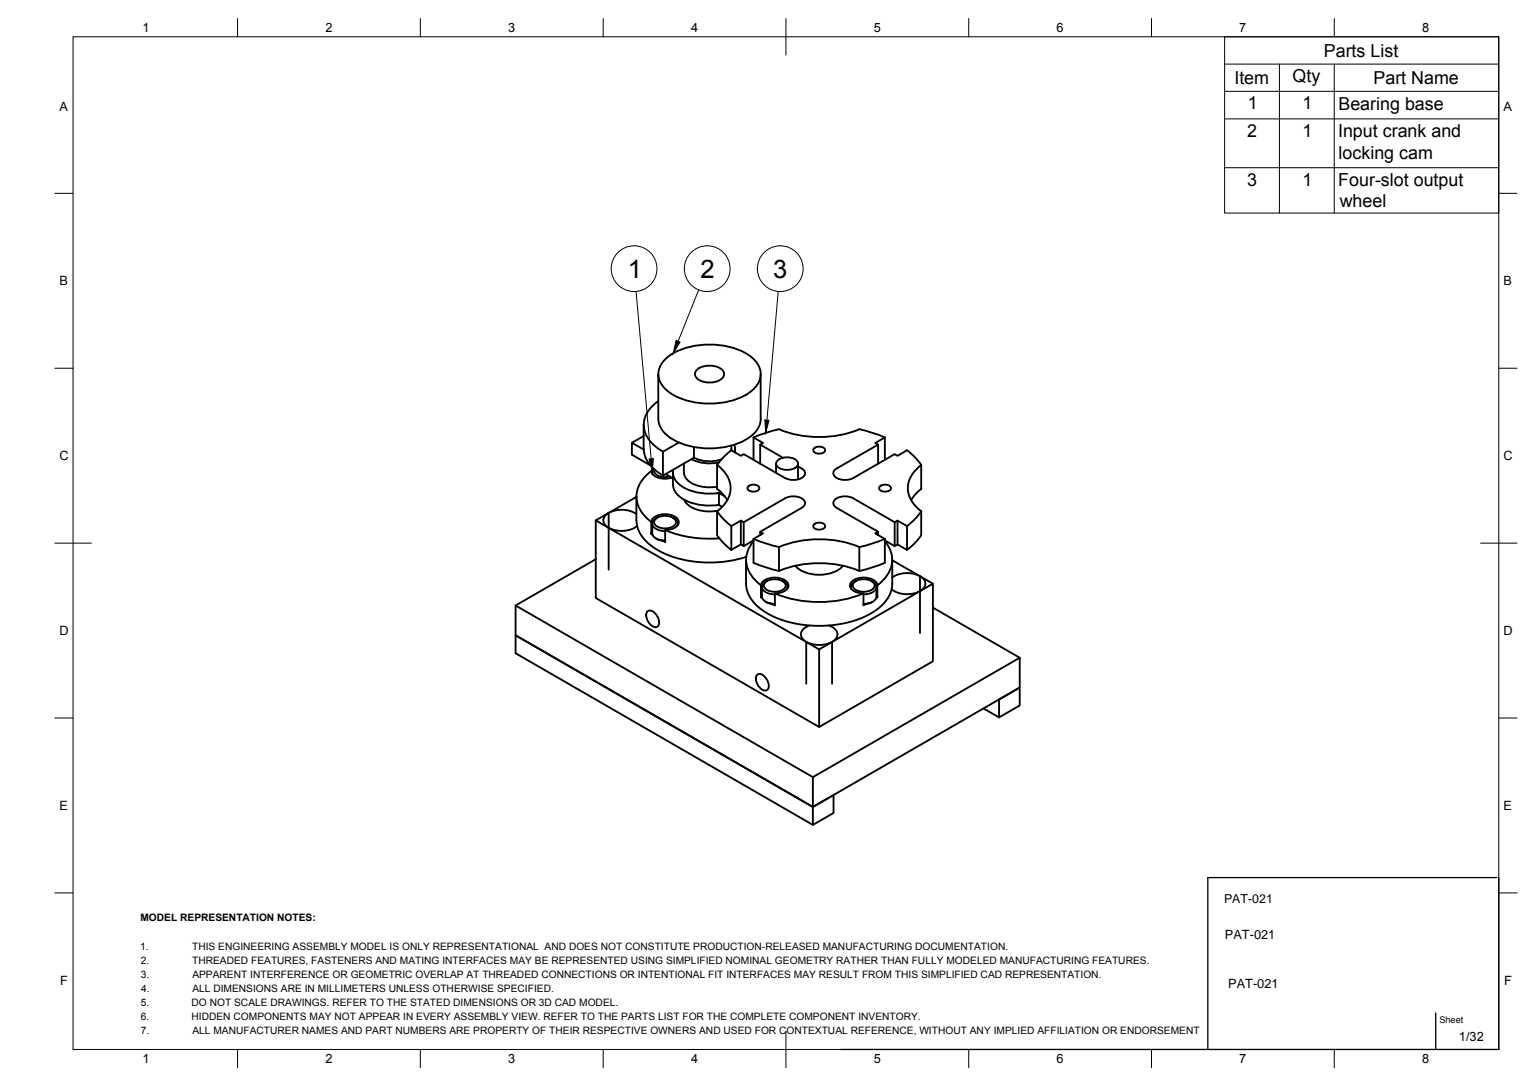
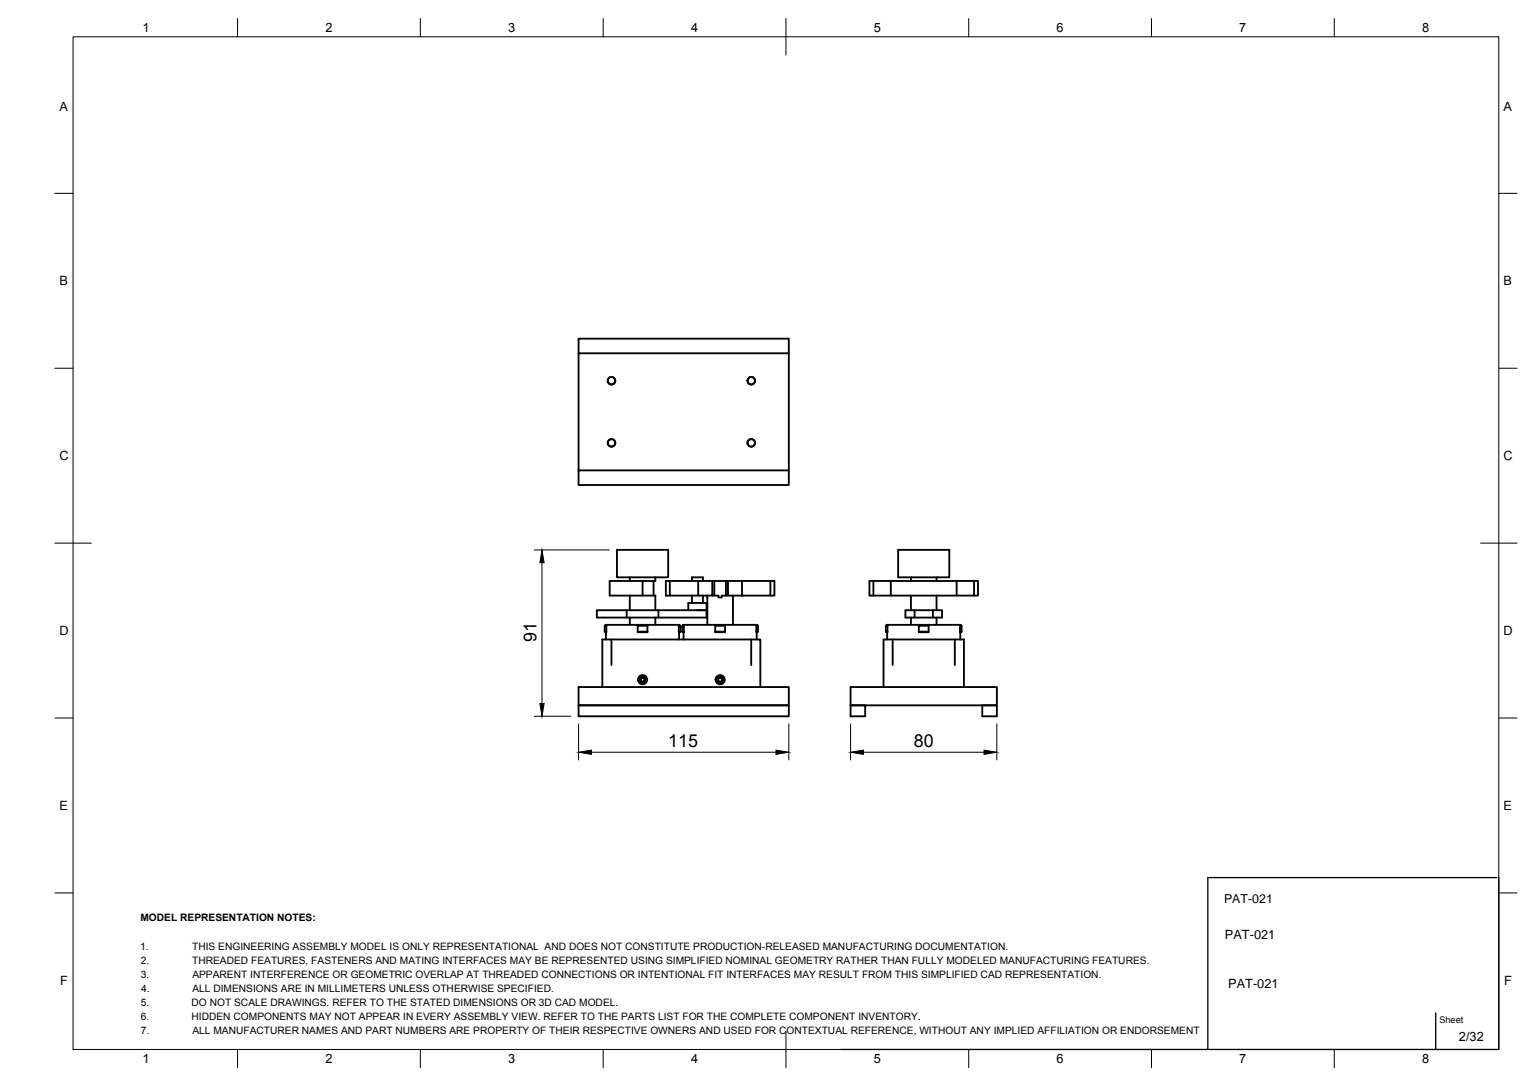
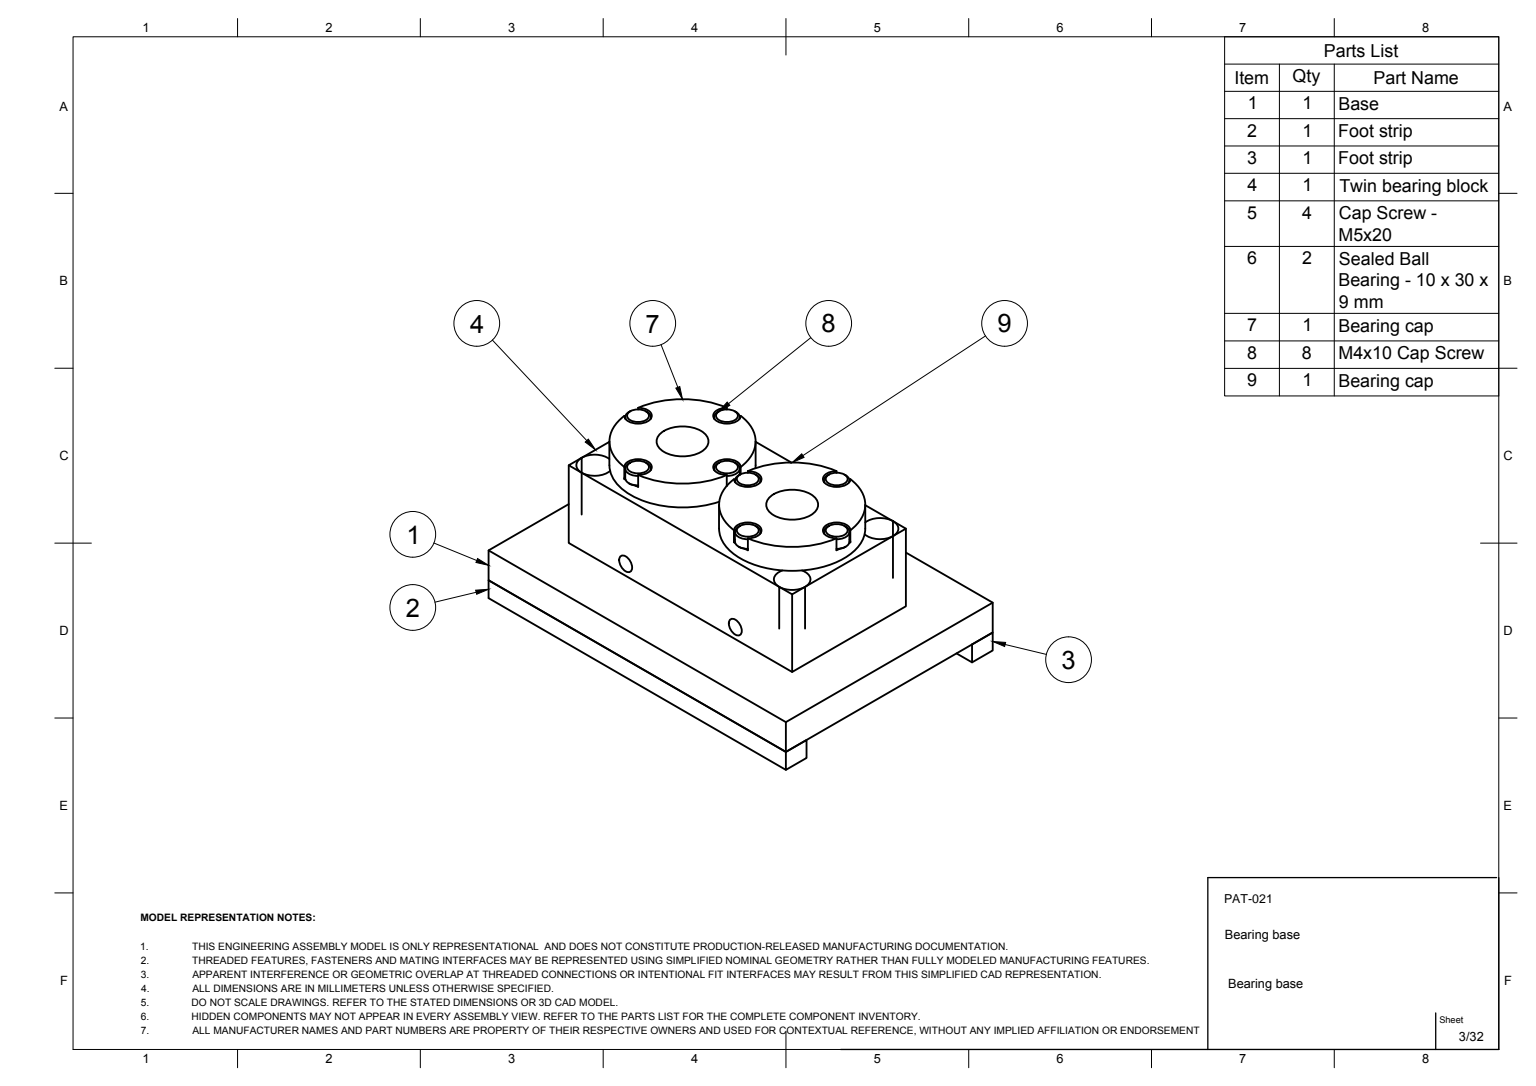
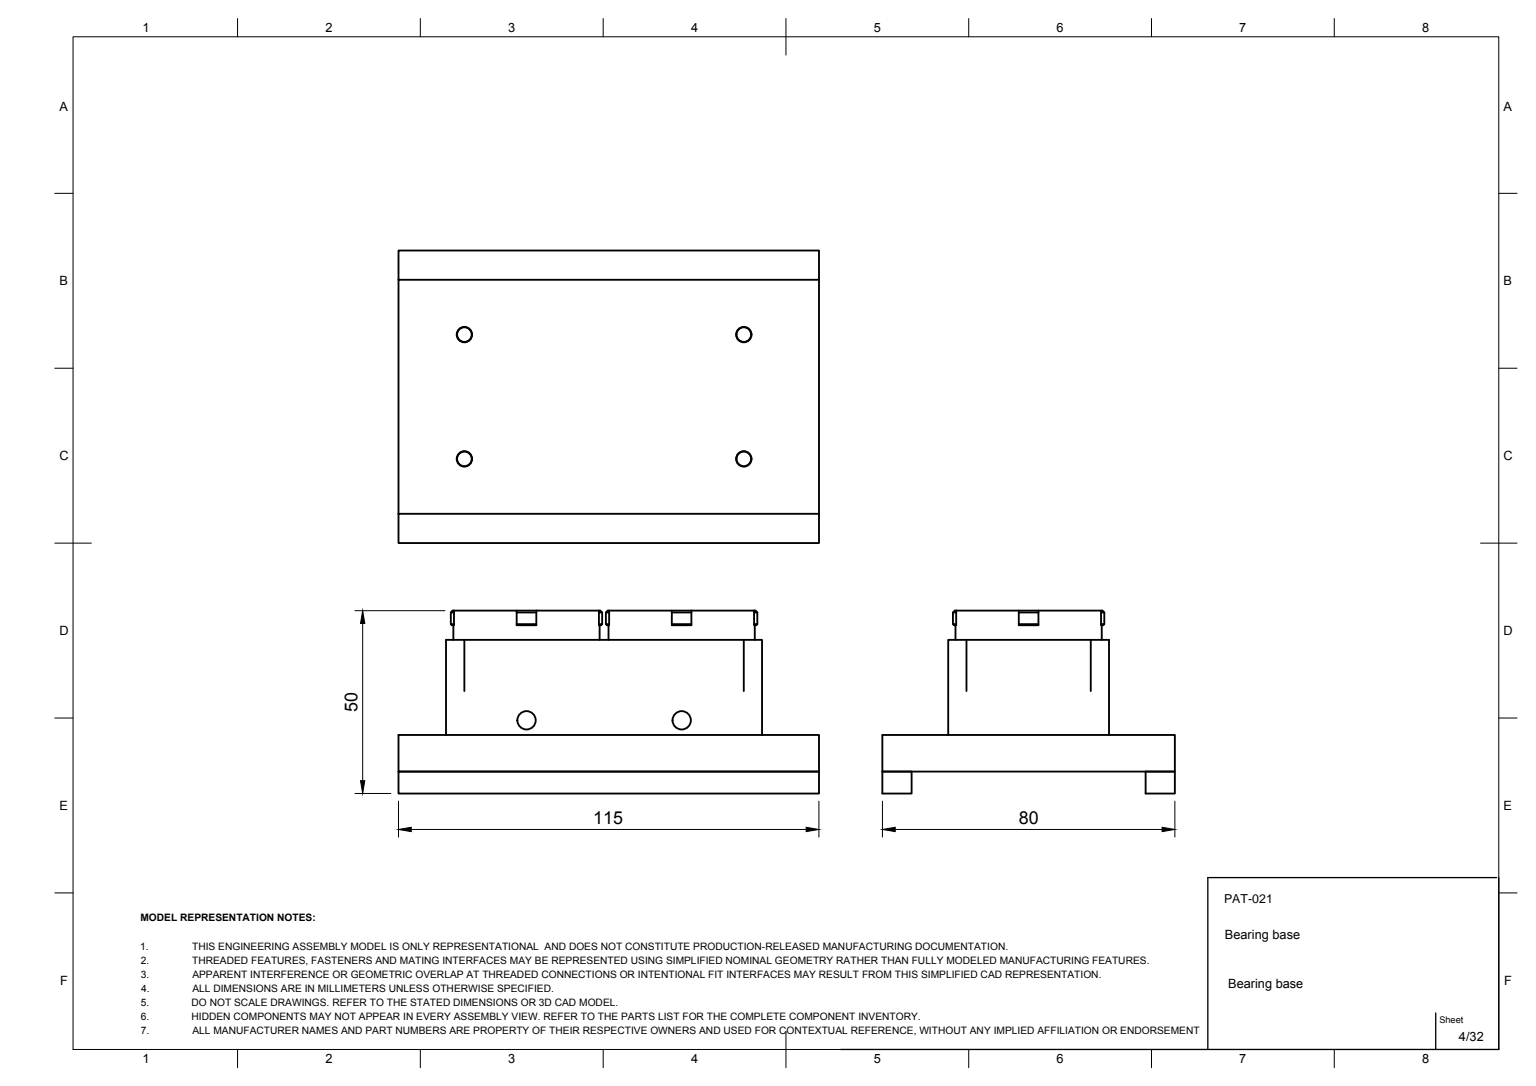
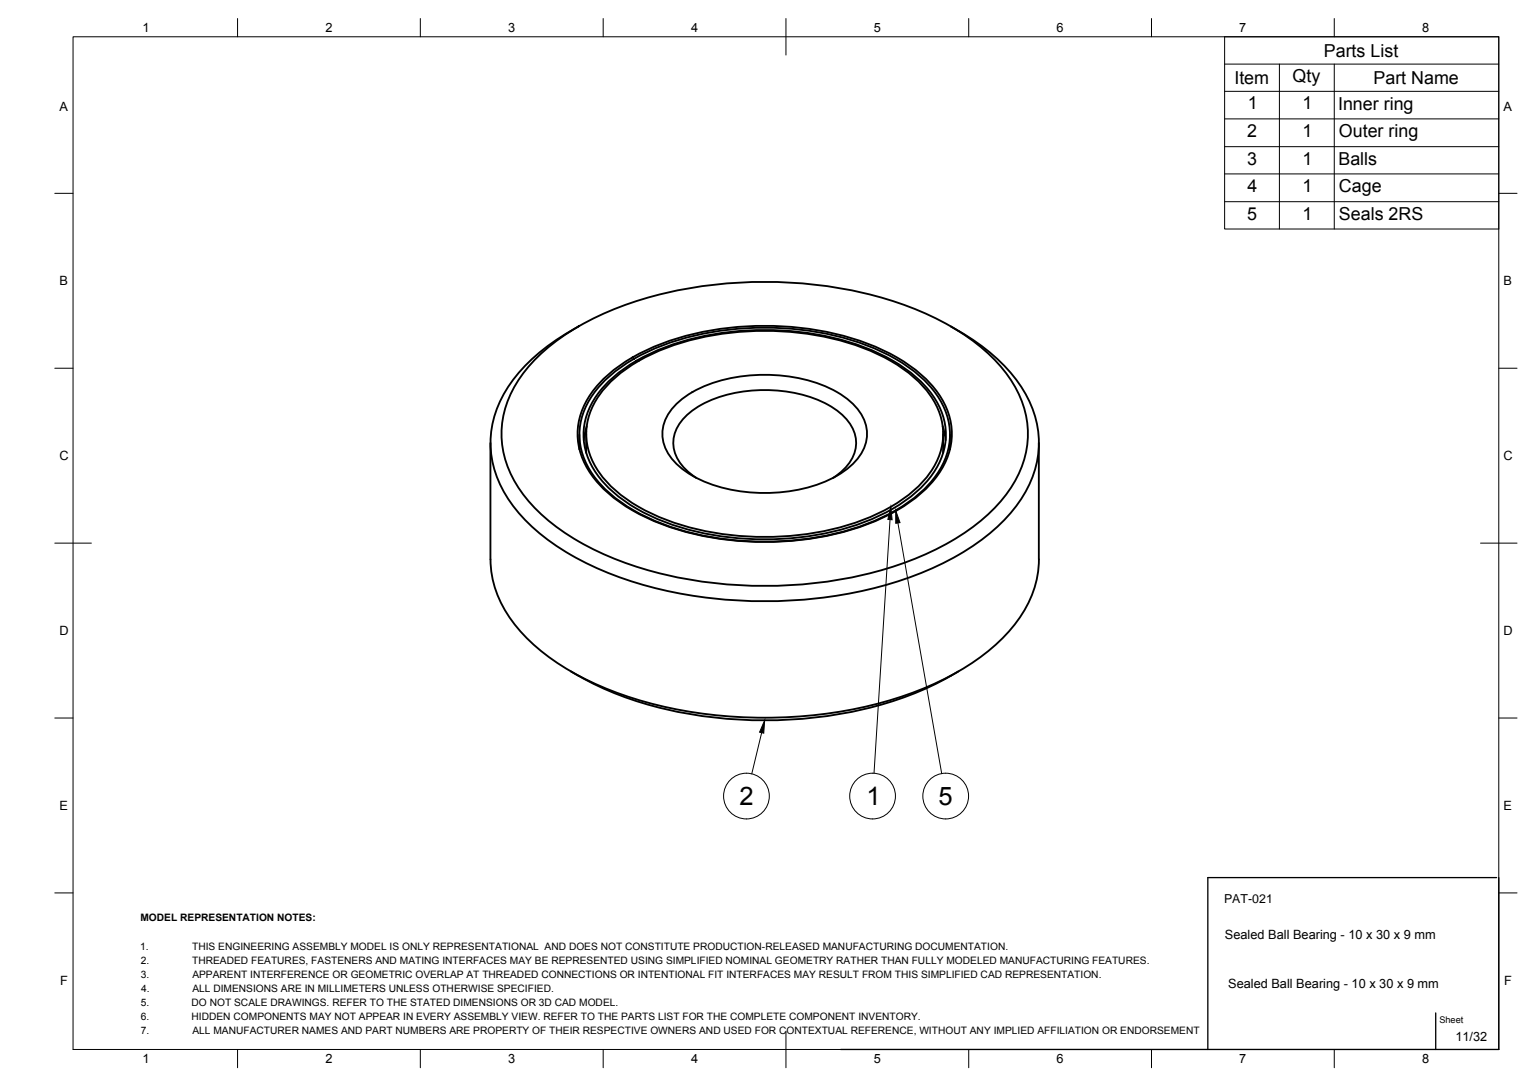
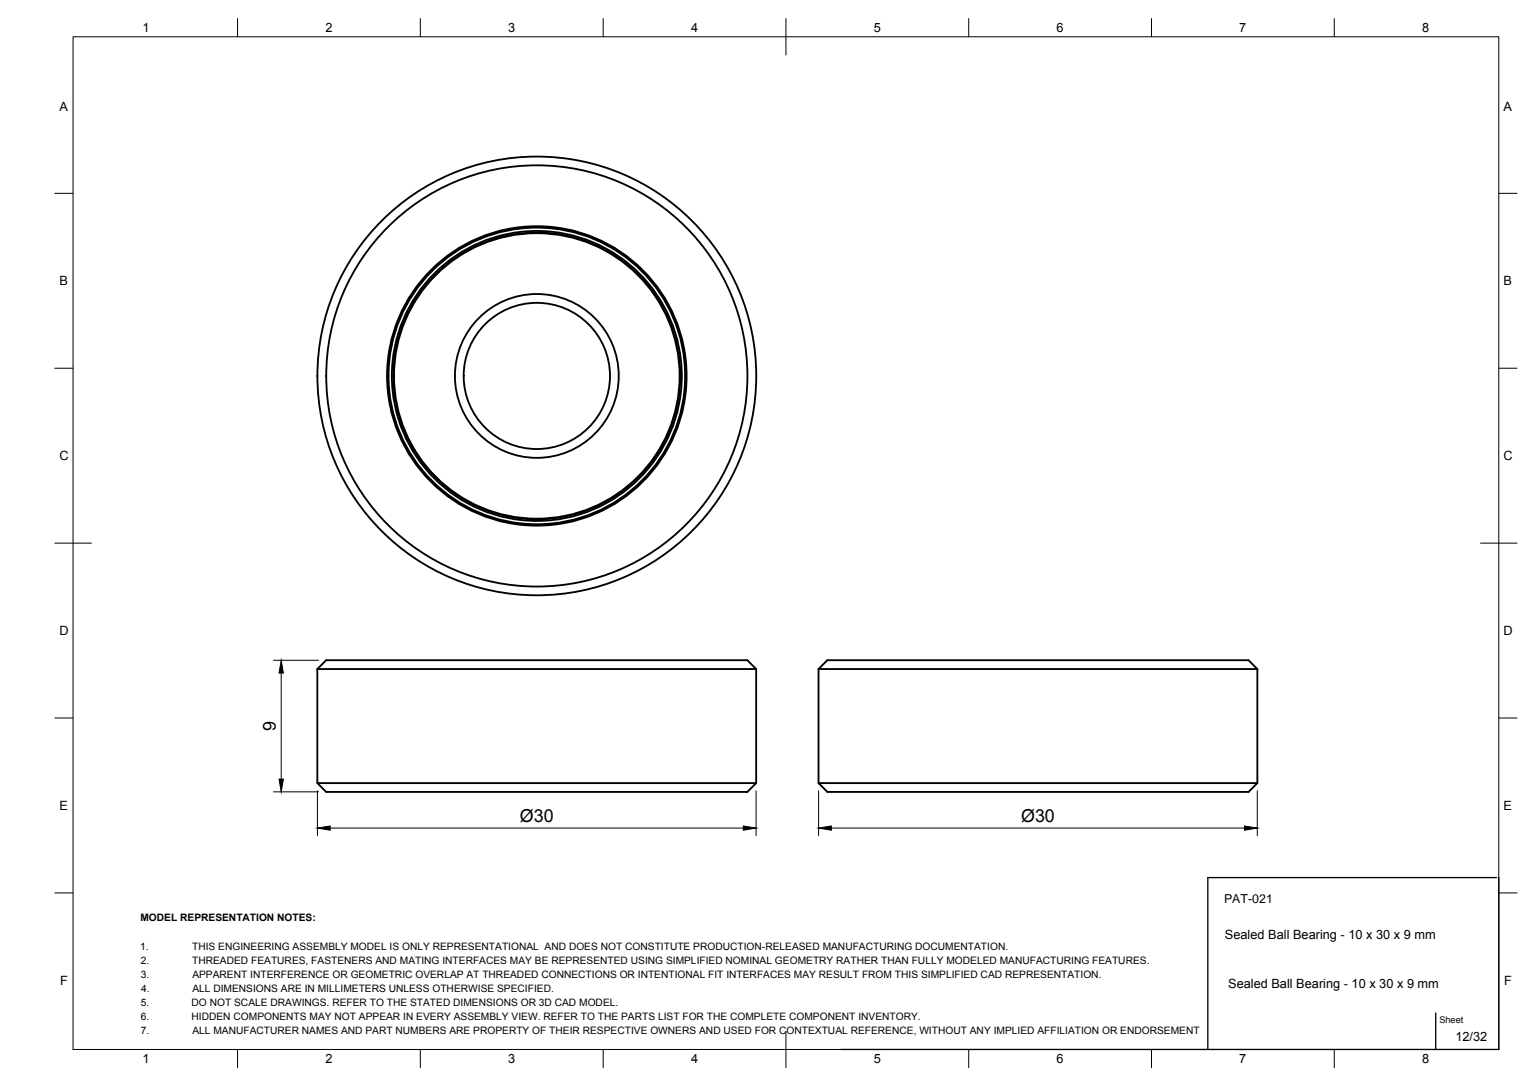
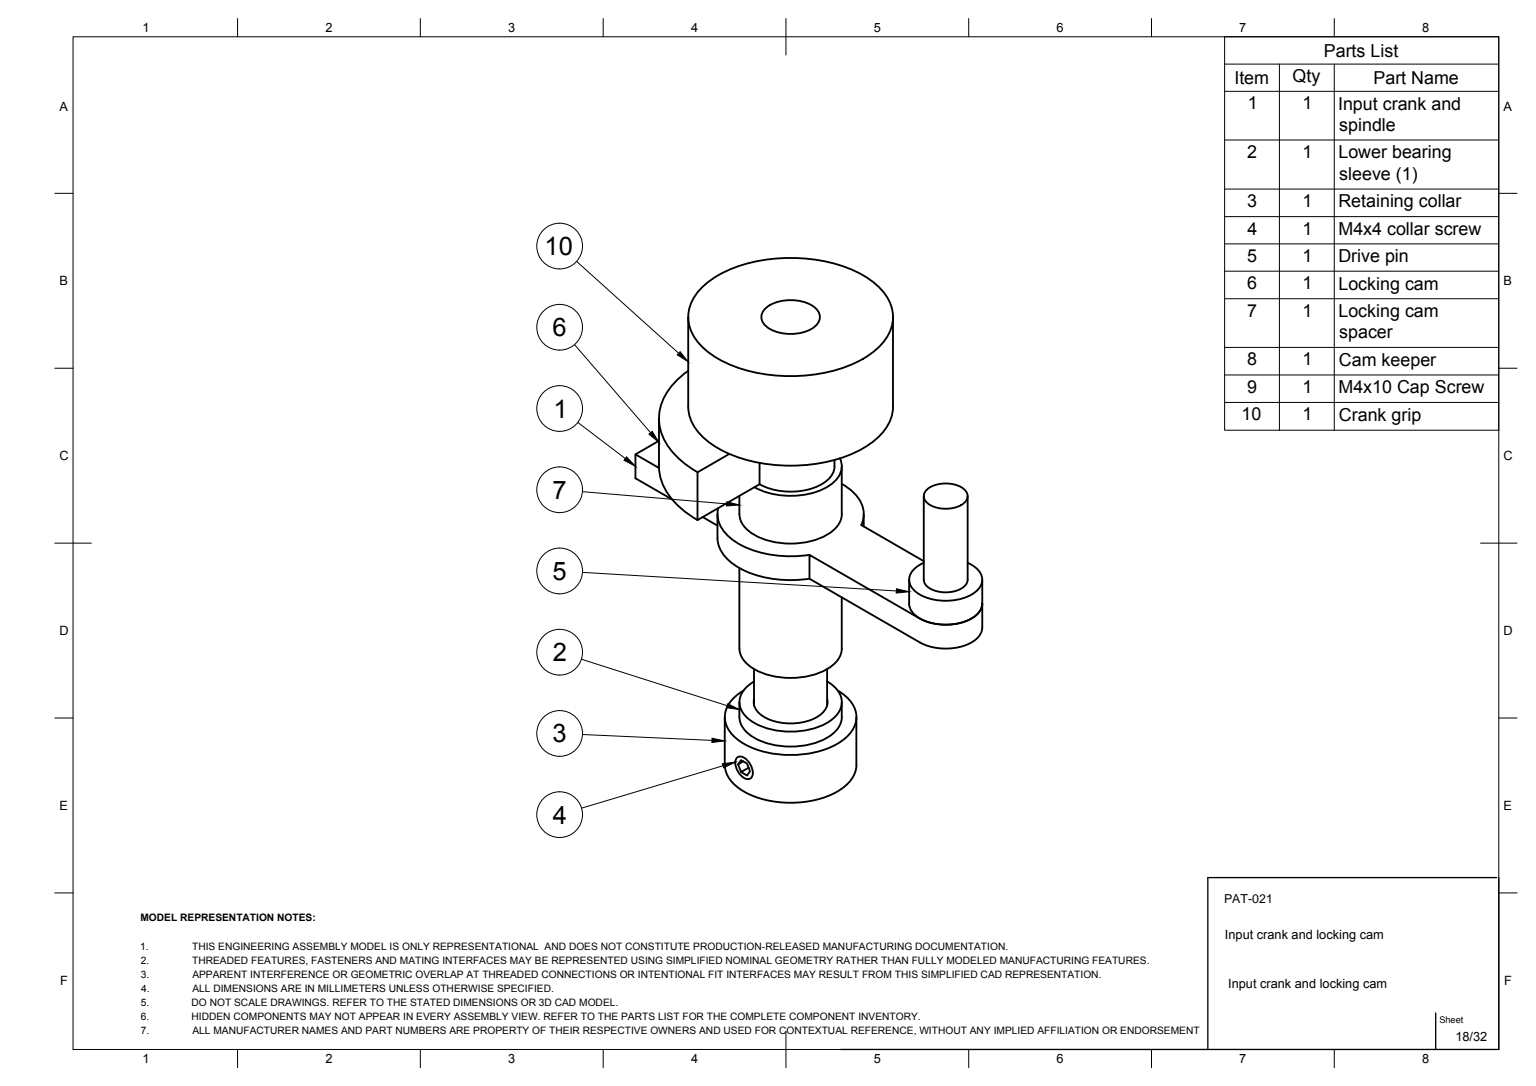
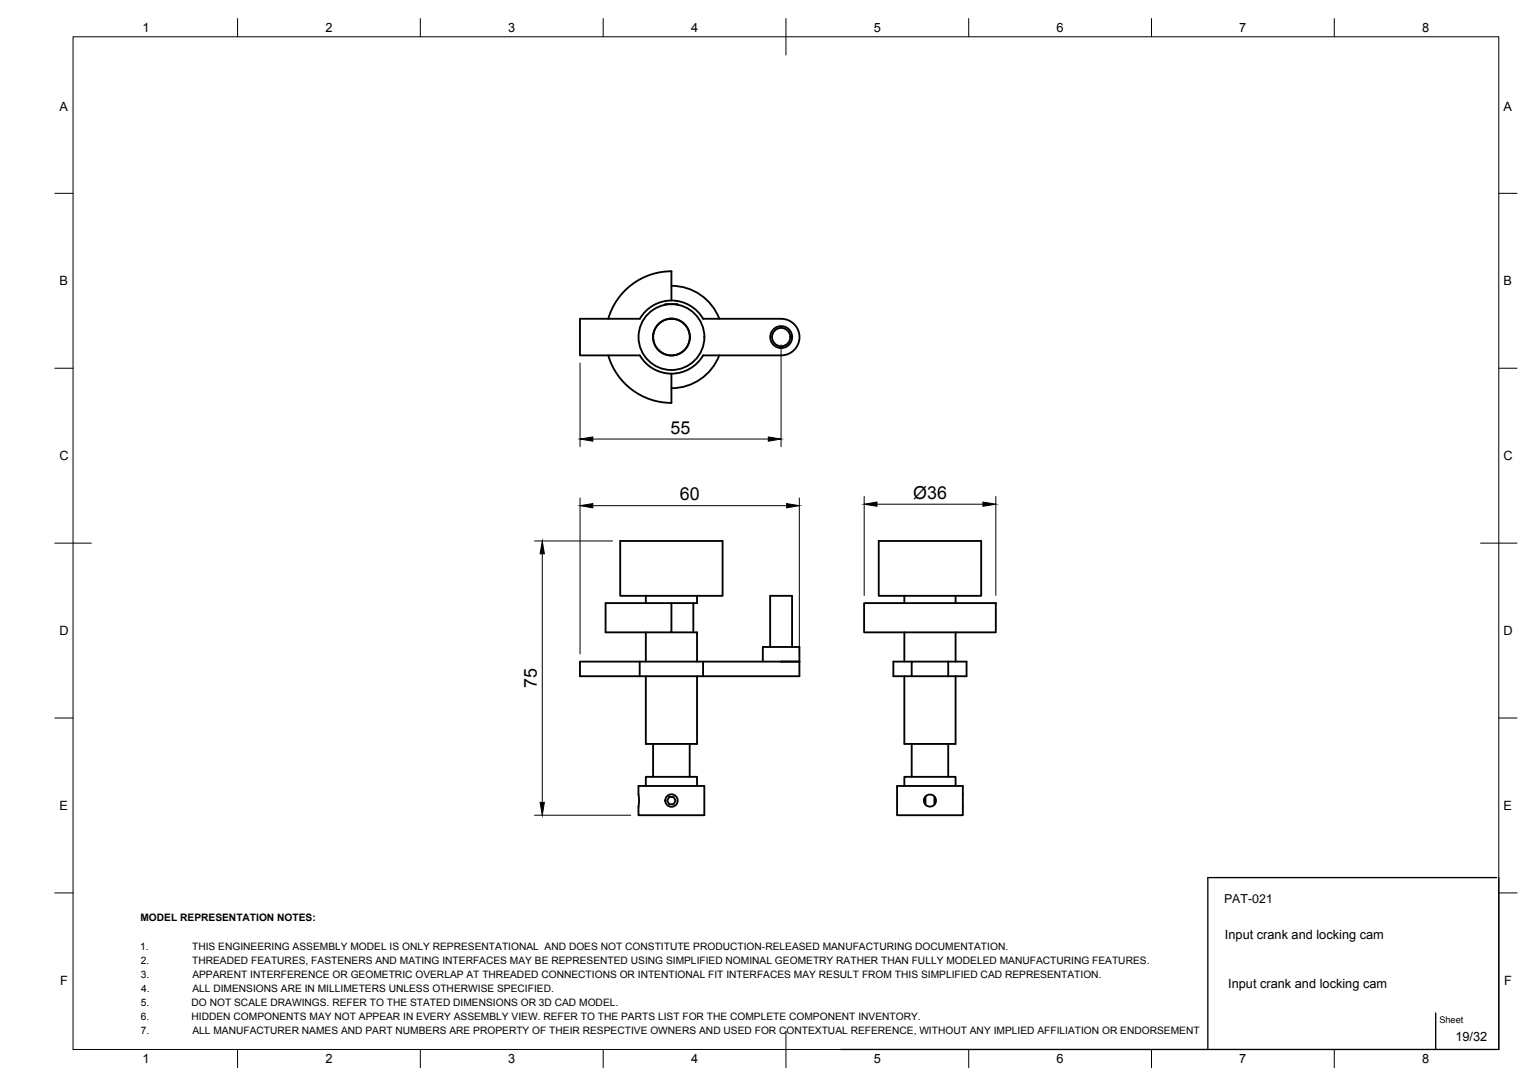
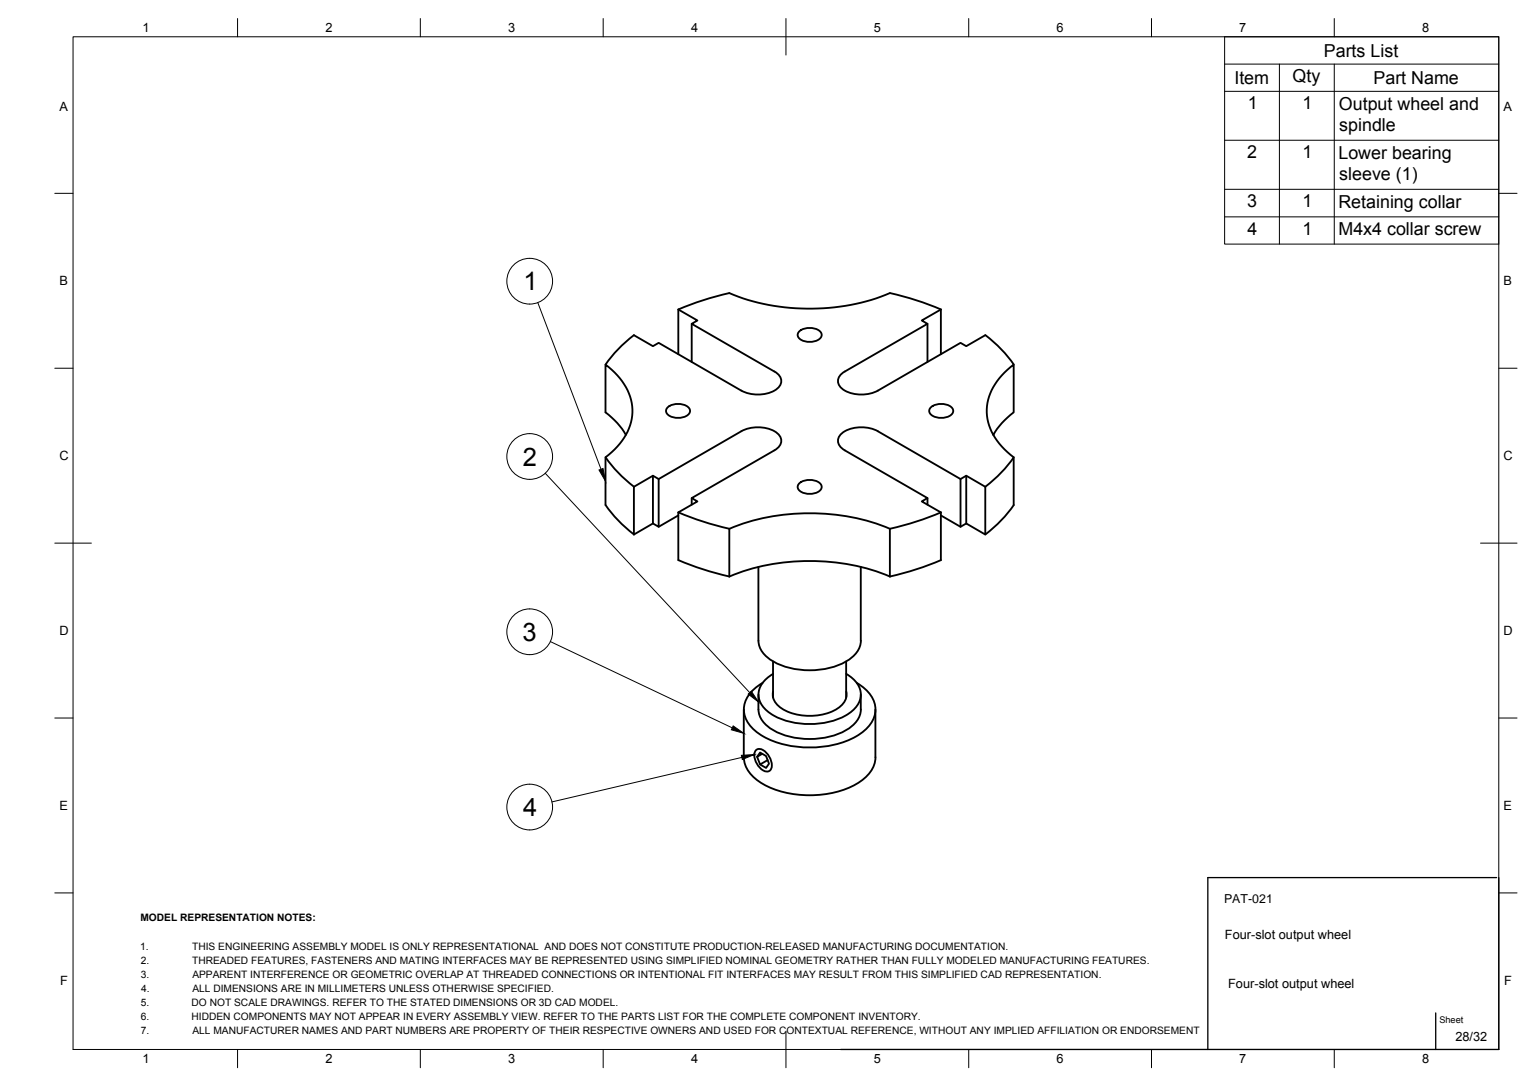
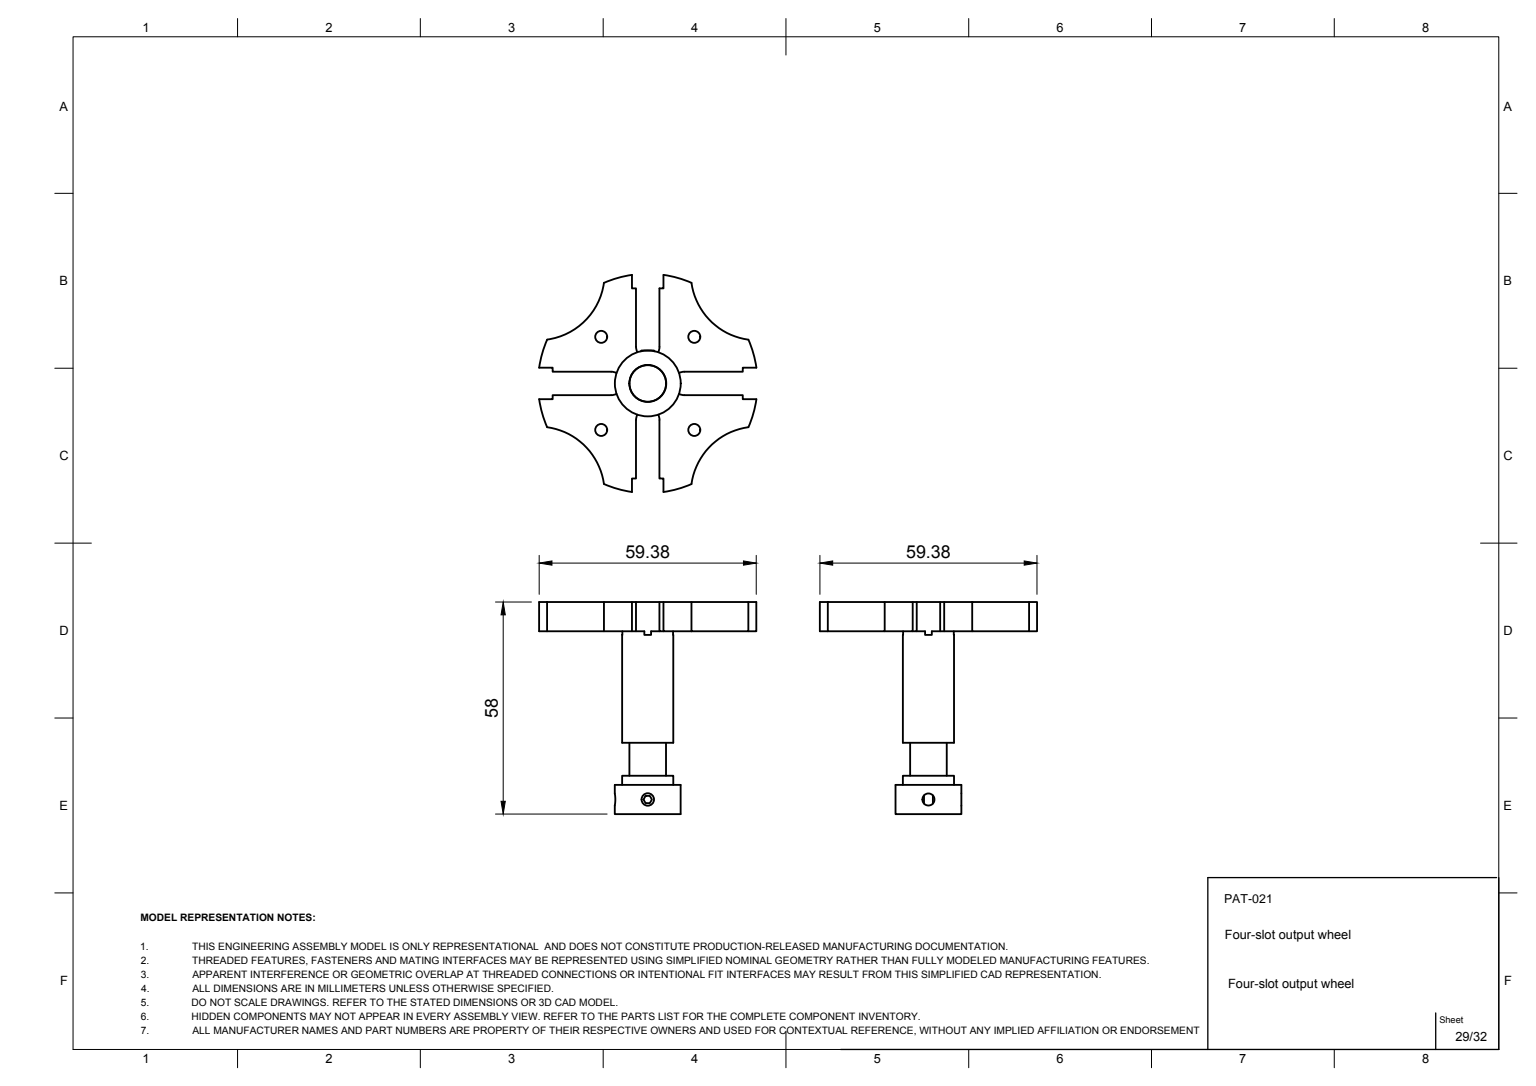
ISO-10303-21;
HEADER;
/* Generated by software containing ST-Developer
 * from STEP Tools, Inc. (www.steptools.com) 
 */

FILE_DESCRIPTION(
/* description */ ('Chain-less indexing wheel (Geneva) drive'),
/* implementation_level */ '2;1');

FILE_NAME(
/* name */ 'PAT-021',
/* time_stamp */ '2026-10-28T03:25:22-07:00',
/* author */ (''),
/* organization */ (''),
/* preprocessor_version */ 'ST-DEVELOPER v20.2',
/* originating_system */ 'Autodesk Translation Framework v15.17.0.0',
/* authorisation */ '');

FILE_SCHEMA (('AUTOMOTIVE_DESIGN { 1 0 10303 214 3 1 1 }'));
ENDSEC;

DATA;
#10=MECHANICAL_DESIGN_GEOMETRIC_PRESENTATION_REPRESENTATION('',(#303,#304,
#305,#306,#307,#308,#309,#310,#311,#312,#313,#314,#315,#316,#317,#318,#319,
#320,#321,#322,#323,#324,#325,#326,#327,#328,#329,#330,#331,#332,#333,#334,
#335),#10957);
#11=ITEM_DEFINED_TRANSFORMATION($,$,#6271,#6399);
#12=ITEM_DEFINED_TRANSFORMATION($,$,#6291,#6400);
#13=ITEM_DEFINED_TRANSFORMATION($,$,#6311,#6401);
#14=ITEM_DEFINED_TRANSFORMATION($,$,#6328,#6402);
#15=ITEM_DEFINED_TRANSFORMATION($,$,#6382,#6403);
#16=ITEM_DEFINED_TRANSFORMATION($,$,#6012,#6549);
#17=ITEM_DEFINED_TRANSFORMATION($,$,#6031,#6550);
#18=ITEM_DEFINED_TRANSFORMATION($,$,#6038,#6551);
#19=ITEM_DEFINED_TRANSFORMATION($,$,#6045,#6552);
#20=ITEM_DEFINED_TRANSFORMATION($,$,#6146,#6553);
#21=ITEM_DEFINED_TRANSFORMATION($,$,#6195,#6554);
#22=ITEM_DEFINED_TRANSFORMATION($,$,#6244,#6555);
#23=ITEM_DEFINED_TRANSFORMATION($,$,#6244,#6556);
#24=ITEM_DEFINED_TRANSFORMATION($,$,#6244,#6557);
#25=ITEM_DEFINED_TRANSFORMATION($,$,#6244,#6558);
#26=ITEM_DEFINED_TRANSFORMATION($,$,#6270,#6559);
#27=ITEM_DEFINED_TRANSFORMATION($,$,#6525,#6560);
#28=ITEM_DEFINED_TRANSFORMATION($,$,#6525,#6561);
#29=ITEM_DEFINED_TRANSFORMATION($,$,#6525,#6562);
#30=ITEM_DEFINED_TRANSFORMATION($,$,#6525,#6563);
#31=ITEM_DEFINED_TRANSFORMATION($,$,#6270,#6564);
#32=ITEM_DEFINED_TRANSFORMATION($,$,#6525,#6565);
#33=ITEM_DEFINED_TRANSFORMATION($,$,#6525,#6566);
#34=ITEM_DEFINED_TRANSFORMATION($,$,#6525,#6567);
#35=ITEM_DEFINED_TRANSFORMATION($,$,#6525,#6568);
#36=ITEM_DEFINED_TRANSFORMATION($,$,#6405,#6732);
#37=ITEM_DEFINED_TRANSFORMATION($,$,#6441,#6733);
#38=ITEM_DEFINED_TRANSFORMATION($,$,#6450,#6734);
#39=ITEM_DEFINED_TRANSFORMATION($,$,#6470,#6735);
#40=ITEM_DEFINED_TRANSFORMATION($,$,#6484,#6736);
#41=ITEM_DEFINED_TRANSFORMATION($,$,#6498,#6737);
#42=ITEM_DEFINED_TRANSFORMATION($,$,#6507,#6738);
#43=ITEM_DEFINED_TRANSFORMATION($,$,#6516,#6739);
#44=ITEM_DEFINED_TRANSFORMATION($,$,#6717,#6740);
#45=ITEM_DEFINED_TRANSFORMATION($,$,#6525,#6741);
#46=ITEM_DEFINED_TRANSFORMATION($,$,#6570,#6742);
#47=ITEM_DEFINED_TRANSFORMATION($,$,#6688,#6743);
#48=ITEM_DEFINED_TRANSFORMATION($,$,#6697,#6744);
#49=ITEM_DEFINED_TRANSFORMATION($,$,#6717,#6745);
#50=ITEM_DEFINED_TRANSFORMATION($,$,#6011,#6746);
#51=ITEM_DEFINED_TRANSFORMATION($,$,#6404,#6747);
#52=ITEM_DEFINED_TRANSFORMATION($,$,#6569,#6748);
#53=(
REPRESENTATION_RELATIONSHIP($,$,#11074,#11073)
REPRESENTATION_RELATIONSHIP_WITH_TRANSFORMATION(#11)
SHAPE_REPRESENTATION_RELATIONSHIP()
);
#54=(
REPRESENTATION_RELATIONSHIP($,$,#11075,#11073)
REPRESENTATION_RELATIONSHIP_WITH_TRANSFORMATION(#12)
SHAPE_REPRESENTATION_RELATIONSHIP()
);
#55=(
REPRESENTATION_RELATIONSHIP($,$,#11076,#11073)
REPRESENTATION_RELATIONSHIP_WITH_TRANSFORMATION(#13)
SHAPE_REPRESENTATION_RELATIONSHIP()
);
#56=(
REPRESENTATION_RELATIONSHIP($,$,#11077,#11073)
REPRESENTATION_RELATIONSHIP_WITH_TRANSFORMATION(#14)
SHAPE_REPRESENTATION_RELATIONSHIP()
);
#57=(
REPRESENTATION_RELATIONSHIP($,$,#11078,#11073)
REPRESENTATION_RELATIONSHIP_WITH_TRANSFORMATION(#15)
SHAPE_REPRESENTATION_RELATIONSHIP()
);
#58=(
REPRESENTATION_RELATIONSHIP($,$,#11066,#11065)
REPRESENTATION_RELATIONSHIP_WITH_TRANSFORMATION(#16)
SHAPE_REPRESENTATION_RELATIONSHIP()
);
#59=(
REPRESENTATION_RELATIONSHIP($,$,#11067,#11065)
REPRESENTATION_RELATIONSHIP_WITH_TRANSFORMATION(#17)
SHAPE_REPRESENTATION_RELATIONSHIP()
);
#60=(
REPRESENTATION_RELATIONSHIP($,$,#11068,#11065)
REPRESENTATION_RELATIONSHIP_WITH_TRANSFORMATION(#18)
SHAPE_REPRESENTATION_RELATIONSHIP()
);
#61=(
REPRESENTATION_RELATIONSHIP($,$,#11069,#11065)
REPRESENTATION_RELATIONSHIP_WITH_TRANSFORMATION(#19)
SHAPE_REPRESENTATION_RELATIONSHIP()
);
#62=(
REPRESENTATION_RELATIONSHIP($,$,#11070,#11065)
REPRESENTATION_RELATIONSHIP_WITH_TRANSFORMATION(#20)
SHAPE_REPRESENTATION_RELATIONSHIP()
);
#63=(
REPRESENTATION_RELATIONSHIP($,$,#11071,#11065)
REPRESENTATION_RELATIONSHIP_WITH_TRANSFORMATION(#21)
SHAPE_REPRESENTATION_RELATIONSHIP()
);
#64=(
REPRESENTATION_RELATIONSHIP($,$,#11072,#11065)
REPRESENTATION_RELATIONSHIP_WITH_TRANSFORMATION(#22)
SHAPE_REPRESENTATION_RELATIONSHIP()
);
#65=(
REPRESENTATION_RELATIONSHIP($,$,#11072,#11065)
REPRESENTATION_RELATIONSHIP_WITH_TRANSFORMATION(#23)
SHAPE_REPRESENTATION_RELATIONSHIP()
);
#66=(
REPRESENTATION_RELATIONSHIP($,$,#11072,#11065)
REPRESENTATION_RELATIONSHIP_WITH_TRANSFORMATION(#24)
SHAPE_REPRESENTATION_RELATIONSHIP()
);
#67=(
REPRESENTATION_RELATIONSHIP($,$,#11072,#11065)
REPRESENTATION_RELATIONSHIP_WITH_TRANSFORMATION(#25)
SHAPE_REPRESENTATION_RELATIONSHIP()
);
#68=(
REPRESENTATION_RELATIONSHIP($,$,#11073,#11065)
REPRESENTATION_RELATIONSHIP_WITH_TRANSFORMATION(#26)
SHAPE_REPRESENTATION_RELATIONSHIP()
);
#69=(
REPRESENTATION_RELATIONSHIP($,$,#11088,#11065)
REPRESENTATION_RELATIONSHIP_WITH_TRANSFORMATION(#27)
SHAPE_REPRESENTATION_RELATIONSHIP()
);
#70=(
REPRESENTATION_RELATIONSHIP($,$,#11088,#11065)
REPRESENTATION_RELATIONSHIP_WITH_TRANSFORMATION(#28)
SHAPE_REPRESENTATION_RELATIONSHIP()
);
#71=(
REPRESENTATION_RELATIONSHIP($,$,#11088,#11065)
REPRESENTATION_RELATIONSHIP_WITH_TRANSFORMATION(#29)
SHAPE_REPRESENTATION_RELATIONSHIP()
);
#72=(
REPRESENTATION_RELATIONSHIP($,$,#11088,#11065)
REPRESENTATION_RELATIONSHIP_WITH_TRANSFORMATION(#30)
SHAPE_REPRESENTATION_RELATIONSHIP()
);
#73=(
REPRESENTATION_RELATIONSHIP($,$,#11073,#11065)
REPRESENTATION_RELATIONSHIP_WITH_TRANSFORMATION(#31)
SHAPE_REPRESENTATION_RELATIONSHIP()
);
#74=(
REPRESENTATION_RELATIONSHIP($,$,#11088,#11065)
REPRESENTATION_RELATIONSHIP_WITH_TRANSFORMATION(#32)
SHAPE_REPRESENTATION_RELATIONSHIP()
);
#75=(
REPRESENTATION_RELATIONSHIP($,$,#11088,#11065)
REPRESENTATION_RELATIONSHIP_WITH_TRANSFORMATION(#33)
SHAPE_REPRESENTATION_RELATIONSHIP()
);
#76=(
REPRESENTATION_RELATIONSHIP($,$,#11088,#11065)
REPRESENTATION_RELATIONSHIP_WITH_TRANSFORMATION(#34)
SHAPE_REPRESENTATION_RELATIONSHIP()
);
#77=(
REPRESENTATION_RELATIONSHIP($,$,#11088,#11065)
REPRESENTATION_RELATIONSHIP_WITH_TRANSFORMATION(#35)
SHAPE_REPRESENTATION_RELATIONSHIP()
);
#78=(
REPRESENTATION_RELATIONSHIP($,$,#11080,#11079)
REPRESENTATION_RELATIONSHIP_WITH_TRANSFORMATION(#36)
SHAPE_REPRESENTATION_RELATIONSHIP()
);
#79=(
REPRESENTATION_RELATIONSHIP($,$,#11081,#11079)
REPRESENTATION_RELATIONSHIP_WITH_TRANSFORMATION(#37)
SHAPE_REPRESENTATION_RELATIONSHIP()
);
#80=(
REPRESENTATION_RELATIONSHIP($,$,#11082,#11079)
REPRESENTATION_RELATIONSHIP_WITH_TRANSFORMATION(#38)
SHAPE_REPRESENTATION_RELATIONSHIP()
);
#81=(
REPRESENTATION_RELATIONSHIP($,$,#11083,#11079)
REPRESENTATION_RELATIONSHIP_WITH_TRANSFORMATION(#39)
SHAPE_REPRESENTATION_RELATIONSHIP()
);
#82=(
REPRESENTATION_RELATIONSHIP($,$,#11084,#11079)
REPRESENTATION_RELATIONSHIP_WITH_TRANSFORMATION(#40)
SHAPE_REPRESENTATION_RELATIONSHIP()
);
#83=(
REPRESENTATION_RELATIONSHIP($,$,#11085,#11079)
REPRESENTATION_RELATIONSHIP_WITH_TRANSFORMATION(#41)
SHAPE_REPRESENTATION_RELATIONSHIP()
);
#84=(
REPRESENTATION_RELATIONSHIP($,$,#11086,#11079)
REPRESENTATION_RELATIONSHIP_WITH_TRANSFORMATION(#42)
SHAPE_REPRESENTATION_RELATIONSHIP()
);
#85=(
REPRESENTATION_RELATIONSHIP($,$,#11087,#11079)
REPRESENTATION_RELATIONSHIP_WITH_TRANSFORMATION(#43)
SHAPE_REPRESENTATION_RELATIONSHIP()
);
#86=(
REPRESENTATION_RELATIONSHIP($,$,#11093,#11079)
REPRESENTATION_RELATIONSHIP_WITH_TRANSFORMATION(#44)
SHAPE_REPRESENTATION_RELATIONSHIP()
);
#87=(
REPRESENTATION_RELATIONSHIP($,$,#11088,#11079)
REPRESENTATION_RELATIONSHIP_WITH_TRANSFORMATION(#45)
SHAPE_REPRESENTATION_RELATIONSHIP()
);
#88=(
REPRESENTATION_RELATIONSHIP($,$,#11090,#11089)
REPRESENTATION_RELATIONSHIP_WITH_TRANSFORMATION(#46)
SHAPE_REPRESENTATION_RELATIONSHIP()
);
#89=(
REPRESENTATION_RELATIONSHIP($,$,#11091,#11089)
REPRESENTATION_RELATIONSHIP_WITH_TRANSFORMATION(#47)
SHAPE_REPRESENTATION_RELATIONSHIP()
);
#90=(
REPRESENTATION_RELATIONSHIP($,$,#11092,#11089)
REPRESENTATION_RELATIONSHIP_WITH_TRANSFORMATION(#48)
SHAPE_REPRESENTATION_RELATIONSHIP()
);
#91=(
REPRESENTATION_RELATIONSHIP($,$,#11093,#11089)
REPRESENTATION_RELATIONSHIP_WITH_TRANSFORMATION(#49)
SHAPE_REPRESENTATION_RELATIONSHIP()
);
#92=(
REPRESENTATION_RELATIONSHIP($,$,#11065,#11064)
REPRESENTATION_RELATIONSHIP_WITH_TRANSFORMATION(#50)
SHAPE_REPRESENTATION_RELATIONSHIP()
);
#93=(
REPRESENTATION_RELATIONSHIP($,$,#11079,#11064)
REPRESENTATION_RELATIONSHIP_WITH_TRANSFORMATION(#51)
SHAPE_REPRESENTATION_RELATIONSHIP()
);
#94=(
REPRESENTATION_RELATIONSHIP($,$,#11089,#11064)
REPRESENTATION_RELATIONSHIP_WITH_TRANSFORMATION(#52)
SHAPE_REPRESENTATION_RELATIONSHIP()
);
#95=CONTEXT_DEPENDENT_SHAPE_REPRESENTATION(#53,#11007);
#96=CONTEXT_DEPENDENT_SHAPE_REPRESENTATION(#54,#11008);
#97=CONTEXT_DEPENDENT_SHAPE_REPRESENTATION(#55,#11009);
#98=CONTEXT_DEPENDENT_SHAPE_REPRESENTATION(#56,#11010);
#99=CONTEXT_DEPENDENT_SHAPE_REPRESENTATION(#57,#11011);
#100=CONTEXT_DEPENDENT_SHAPE_REPRESENTATION(#58,#11022);
#101=CONTEXT_DEPENDENT_SHAPE_REPRESENTATION(#59,#11023);
#102=CONTEXT_DEPENDENT_SHAPE_REPRESENTATION(#60,#11024);
#103=CONTEXT_DEPENDENT_SHAPE_REPRESENTATION(#61,#11025);
#104=CONTEXT_DEPENDENT_SHAPE_REPRESENTATION(#62,#11026);
#105=CONTEXT_DEPENDENT_SHAPE_REPRESENTATION(#63,#11027);
#106=CONTEXT_DEPENDENT_SHAPE_REPRESENTATION(#64,#11028);
#107=CONTEXT_DEPENDENT_SHAPE_REPRESENTATION(#65,#11029);
#108=CONTEXT_DEPENDENT_SHAPE_REPRESENTATION(#66,#11030);
#109=CONTEXT_DEPENDENT_SHAPE_REPRESENTATION(#67,#11031);
#110=CONTEXT_DEPENDENT_SHAPE_REPRESENTATION(#68,#11032);
#111=CONTEXT_DEPENDENT_SHAPE_REPRESENTATION(#69,#11033);
#112=CONTEXT_DEPENDENT_SHAPE_REPRESENTATION(#70,#11034);
#113=CONTEXT_DEPENDENT_SHAPE_REPRESENTATION(#71,#11035);
#114=CONTEXT_DEPENDENT_SHAPE_REPRESENTATION(#72,#11036);
#115=CONTEXT_DEPENDENT_SHAPE_REPRESENTATION(#73,#11037);
#116=CONTEXT_DEPENDENT_SHAPE_REPRESENTATION(#74,#11038);
#117=CONTEXT_DEPENDENT_SHAPE_REPRESENTATION(#75,#11039);
#118=CONTEXT_DEPENDENT_SHAPE_REPRESENTATION(#76,#11040);
#119=CONTEXT_DEPENDENT_SHAPE_REPRESENTATION(#77,#11041);
#120=CONTEXT_DEPENDENT_SHAPE_REPRESENTATION(#78,#11047);
#121=CONTEXT_DEPENDENT_SHAPE_REPRESENTATION(#79,#11048);
#122=CONTEXT_DEPENDENT_SHAPE_REPRESENTATION(#80,#11049);
#123=CONTEXT_DEPENDENT_SHAPE_REPRESENTATION(#81,#11050);
#124=CONTEXT_DEPENDENT_SHAPE_REPRESENTATION(#82,#11051);
#125=CONTEXT_DEPENDENT_SHAPE_REPRESENTATION(#83,#11052);
#126=CONTEXT_DEPENDENT_SHAPE_REPRESENTATION(#84,#11053);
#127=CONTEXT_DEPENDENT_SHAPE_REPRESENTATION(#85,#11054);
#128=CONTEXT_DEPENDENT_SHAPE_REPRESENTATION(#86,#11055);
#129=CONTEXT_DEPENDENT_SHAPE_REPRESENTATION(#87,#11056);
#130=CONTEXT_DEPENDENT_SHAPE_REPRESENTATION(#88,#11057);
#131=CONTEXT_DEPENDENT_SHAPE_REPRESENTATION(#89,#11058);
#132=CONTEXT_DEPENDENT_SHAPE_REPRESENTATION(#90,#11059);
#133=CONTEXT_DEPENDENT_SHAPE_REPRESENTATION(#91,#11060);
#134=CONTEXT_DEPENDENT_SHAPE_REPRESENTATION(#92,#11061);
#135=CONTEXT_DEPENDENT_SHAPE_REPRESENTATION(#93,#11062);
#136=CONTEXT_DEPENDENT_SHAPE_REPRESENTATION(#94,#11063);
#137=NEXT_ASSEMBLY_USAGE_OCCURRENCE('Inner ring:1','Inner ring:1',
'Inner ring:1',#11104,#11105,'Inner ring:1');
#138=NEXT_ASSEMBLY_USAGE_OCCURRENCE('Outer ring:1','Outer ring:1',
'Outer ring:1',#11104,#11106,'Outer ring:1');
#139=NEXT_ASSEMBLY_USAGE_OCCURRENCE('Balls:1','Balls:1','Balls:1',#11104,
#11107,'Balls:1');
#140=NEXT_ASSEMBLY_USAGE_OCCURRENCE('Cage:1','Cage:1','Cage:1',#11104,#11108,
'Cage:1');
#141=NEXT_ASSEMBLY_USAGE_OCCURRENCE('Seals 2RS:1','Seals 2RS:1',
'Seals 2RS:1',#11104,#11109,'Seals 2RS:1');
#142=NEXT_ASSEMBLY_USAGE_OCCURRENCE('Base:1','Base:1','Base:1',#11096,#11097,
'Base:1');
#143=NEXT_ASSEMBLY_USAGE_OCCURRENCE('Foot strip:1','Foot strip:1',
'Foot strip:1',#11096,#11098,'Foot strip:1');
#144=NEXT_ASSEMBLY_USAGE_OCCURRENCE('Foot strip (1):1',
'Foot strip (1):1','Foot strip (1):1',#11096,#11099,'Foot strip (1):1');
#145=NEXT_ASSEMBLY_USAGE_OCCURRENCE('Twin bearing block:1',
'Twin bearing block:1','Twin bearing block:1',#11096,#11100,
'Twin bearing block:1');
#146=NEXT_ASSEMBLY_USAGE_OCCURRENCE('Bearing cap:1','Bearing cap:1',
'Bearing cap:1',#11096,#11101,'Bearing cap:1');
#147=NEXT_ASSEMBLY_USAGE_OCCURRENCE('Bearing cap (1):1',
'Bearing cap (1):1','Bearing cap (1):1',#11096,#11102,
'Bearing cap (1):1');
#148=NEXT_ASSEMBLY_USAGE_OCCURRENCE('Cap Screw - M5x20:2',
'Cap Screw - M5x20:2','Cap Screw - M5x20:2',#11096,#11103,
'Cap Screw - M5x20:2');
#149=NEXT_ASSEMBLY_USAGE_OCCURRENCE('Cap Screw - M5x20:3',
'Cap Screw - M5x20:3','Cap Screw - M5x20:3',#11096,#11103,
'Cap Screw - M5x20:3');
#150=NEXT_ASSEMBLY_USAGE_OCCURRENCE('Cap Screw - M5x20:4',
'Cap Screw - M5x20:4','Cap Screw - M5x20:4',#11096,#11103,
'Cap Screw - M5x20:4');
#151=NEXT_ASSEMBLY_USAGE_OCCURRENCE('Cap Screw - M5x20:5',
'Cap Screw - M5x20:5','Cap Screw - M5x20:5',#11096,#11103,
'Cap Screw - M5x20:5');
#152=NEXT_ASSEMBLY_USAGE_OCCURRENCE(
'Sealed Ball Bearing - 10 x 30 x 9 mm:2',
'Sealed Ball Bearing - 10 x 30 x 9 mm:2',
'Sealed Ball Bearing - 10 x 30 x 9 mm:2',#11096,#11104,
'Sealed Ball Bearing - 10 x 30 x 9 mm:2');
#153=NEXT_ASSEMBLY_USAGE_OCCURRENCE('M4x10 Cap Screw:2',
'M4x10 Cap Screw:2','M4x10 Cap Screw:2',#11096,#11119,
'M4x10 Cap Screw:2');
#154=NEXT_ASSEMBLY_USAGE_OCCURRENCE('M4x10 Cap Screw:3',
'M4x10 Cap Screw:3','M4x10 Cap Screw:3',#11096,#11119,
'M4x10 Cap Screw:3');
#155=NEXT_ASSEMBLY_USAGE_OCCURRENCE('M4x10 Cap Screw:4',
'M4x10 Cap Screw:4','M4x10 Cap Screw:4',#11096,#11119,
'M4x10 Cap Screw:4');
#156=NEXT_ASSEMBLY_USAGE_OCCURRENCE('M4x10 Cap Screw:5',
'M4x10 Cap Screw:5','M4x10 Cap Screw:5',#11096,#11119,
'M4x10 Cap Screw:5');
#157=NEXT_ASSEMBLY_USAGE_OCCURRENCE(
'Sealed Ball Bearing - 10 x 30 x 9 mm:3',
'Sealed Ball Bearing - 10 x 30 x 9 mm:3',
'Sealed Ball Bearing - 10 x 30 x 9 mm:3',#11096,#11104,
'Sealed Ball Bearing - 10 x 30 x 9 mm:3');
#158=NEXT_ASSEMBLY_USAGE_OCCURRENCE('M4x10 Cap Screw:7',
'M4x10 Cap Screw:7','M4x10 Cap Screw:7',#11096,#11119,
'M4x10 Cap Screw:7');
#159=NEXT_ASSEMBLY_USAGE_OCCURRENCE('M4x10 Cap Screw:8',
'M4x10 Cap Screw:8','M4x10 Cap Screw:8',#11096,#11119,
'M4x10 Cap Screw:8');
#160=NEXT_ASSEMBLY_USAGE_OCCURRENCE('M4x10 Cap Screw:9',
'M4x10 Cap Screw:9','M4x10 Cap Screw:9',#11096,#11119,
'M4x10 Cap Screw:9');
#161=NEXT_ASSEMBLY_USAGE_OCCURRENCE('M4x10 Cap Screw:10',
'M4x10 Cap Screw:10','M4x10 Cap Screw:10',#11096,#11119,
'M4x10 Cap Screw:10');
#162=NEXT_ASSEMBLY_USAGE_OCCURRENCE('Input crank and spindle:1',
'Input crank and spindle:1','Input crank and spindle:1',#11110,#11111,
'Input crank and spindle:1');
#163=NEXT_ASSEMBLY_USAGE_OCCURRENCE('Lower bearing sleeve:1',
'Lower bearing sleeve:1','Lower bearing sleeve:1',#11110,#11112,
'Lower bearing sleeve:1');
#164=NEXT_ASSEMBLY_USAGE_OCCURRENCE('Retaining collar:1',
'Retaining collar:1','Retaining collar:1',#11110,#11113,
'Retaining collar:1');
#165=NEXT_ASSEMBLY_USAGE_OCCURRENCE('Drive pin:1','Drive pin:1',
'Drive pin:1',#11110,#11114,'Drive pin:1');
#166=NEXT_ASSEMBLY_USAGE_OCCURRENCE('Locking cam:1','Locking cam:1',
'Locking cam:1',#11110,#11115,'Locking cam:1');
#167=NEXT_ASSEMBLY_USAGE_OCCURRENCE('Locking cam spacer:1',
'Locking cam spacer:1','Locking cam spacer:1',#11110,#11116,
'Locking cam spacer:1');
#168=NEXT_ASSEMBLY_USAGE_OCCURRENCE('Cam keeper:1','Cam keeper:1',
'Cam keeper:1',#11110,#11117,'Cam keeper:1');
#169=NEXT_ASSEMBLY_USAGE_OCCURRENCE('Crank grip:1','Crank grip:1',
'Crank grip:1',#11110,#11118,'Crank grip:1');
#170=NEXT_ASSEMBLY_USAGE_OCCURRENCE('M4x4 collar screw:2',
'M4x4 collar screw:2','M4x4 collar screw:2',#11110,#11124,
'M4x4 collar screw:2');
#171=NEXT_ASSEMBLY_USAGE_OCCURRENCE('M4x10 Cap Screw:6',
'M4x10 Cap Screw:6','M4x10 Cap Screw:6',#11110,#11119,
'M4x10 Cap Screw:6');
#172=NEXT_ASSEMBLY_USAGE_OCCURRENCE('Output wheel and spindle:1',
'Output wheel and spindle:1','Output wheel and spindle:1',#11120,#11121,
'Output wheel and spindle:1');
#173=NEXT_ASSEMBLY_USAGE_OCCURRENCE('Lower bearing sleeve (1):1',
'Lower bearing sleeve (1):1','Lower bearing sleeve (1):1',#11120,#11122,
'Lower bearing sleeve (1):1');
#174=NEXT_ASSEMBLY_USAGE_OCCURRENCE('Retaining collar (1):1',
'Retaining collar (1):1','Retaining collar (1):1',#11120,#11123,
'Retaining collar (1):1');
#175=NEXT_ASSEMBLY_USAGE_OCCURRENCE('M4x4 collar screw:3',
'M4x4 collar screw:3','M4x4 collar screw:3',#11120,#11124,
'M4x4 collar screw:3');
#176=NEXT_ASSEMBLY_USAGE_OCCURRENCE('Bearing base:1','Bearing base:1',
'Bearing base:1',#11095,#11096,'Bearing base:1');
#177=NEXT_ASSEMBLY_USAGE_OCCURRENCE('Input crank and locking cam:1',
'Input crank and locking cam:1','Input crank and locking cam:1',#11095,
#11110,'Input crank and locking cam:1');
#178=NEXT_ASSEMBLY_USAGE_OCCURRENCE('Four-slot output wheel:1',
'Four-slot output wheel:1','Four-slot output wheel:1',#11095,#11120,
'Four-slot output wheel:1');
#179=SPHERICAL_SURFACE('',#6312,0.23815);
#180=SPHERICAL_SURFACE('',#6314,0.23815);
#181=SPHERICAL_SURFACE('',#6316,0.23815);
#182=SPHERICAL_SURFACE('',#6318,0.23815);
#183=SPHERICAL_SURFACE('',#6320,0.23815);
#184=SPHERICAL_SURFACE('',#6322,0.23815);
#185=SPHERICAL_SURFACE('',#6324,0.23815);
#186=SPHERICAL_SURFACE('',#6326,0.23815);
#187=SPHERICAL_SURFACE('',#6329,0.247676);
#188=SPHERICAL_SURFACE('',#6345,0.247676);
#189=SPHERICAL_SURFACE('',#6350,0.247676);
#190=SPHERICAL_SURFACE('',#6355,0.247676);
#191=SPHERICAL_SURFACE('',#6360,0.247676);
#192=SPHERICAL_SURFACE('',#6365,0.247676);
#193=SPHERICAL_SURFACE('',#6370,0.247676);
#194=SPHERICAL_SURFACE('',#6378,0.247676);
#195=TOROIDAL_SURFACE('',#6272,1.,0.247676);
#196=TOROIDAL_SURFACE('',#6292,1.,0.247676);
#197=ORIENTED_CLOSED_SHELL('',*,#5706,.F.);
#198=ORIENTED_CLOSED_SHELL('',*,#5728,.F.);
#199=CONICAL_SURFACE('',#6247,0.4,0.785398163397448);
#200=CONICAL_SURFACE('',#6251,0.41,0.785398163397448);
#201=CONICAL_SURFACE('',#6255,0.26,0.463647609000806);
#202=CONICAL_SURFACE('',#6259,0.225,0.785398163397448);
#203=CONICAL_SURFACE('',#6283,0.53,0.785398163397448);
#204=CONICAL_SURFACE('',#6290,0.53,0.785398163397448);
#205=CONICAL_SURFACE('',#6303,1.47,0.785398163397449);
#206=CONICAL_SURFACE('',#6307,1.47,0.785398163397449);
#207=CONICAL_SURFACE('',#6538,0.325,0.785398163397448);
#208=CONICAL_SURFACE('',#6542,0.335,0.785398163397448);
#209=CONICAL_SURFACE('',#6546,0.21,0.463647609000806);
#210=CONICAL_SURFACE('',#6729,0.185,0.785398163397449);
#211=BREP_WITH_VOIDS('Body1',#5705,(#197));
#212=BREP_WITH_VOIDS('Body1',#5729,(#198));
#213=B_SPLINE_CURVE_WITH_KNOTS('',3,(#8714,#8715,#8716,#8717,#8718,#8719,
#8720,#8721,#8722,#8723,#8724,#8725,#8726,#8727,#8728,#8729,#8730,#8731,
#8732,#8733,#8734,#8735,#8736,#8737,#8738,#8739,#8740,#8741,#8742,#8743,
#8744,#8745,#8746,#8747),.UNSPECIFIED.,.T.,.F.,(4,2,2,2,2,2,2,2,2,2,2,2,
2,2,2,2,4),(0.,0.094594182476448,0.189188364952896,0.283770357603024,0.378352350253152,
0.472934342903279,0.567516335553407,0.662110518029855,0.756704700506303,
0.851298882982751,0.945893065459199,1.04047505810933,1.13505705075945,1.22963904340958,
1.32422103605971,1.41881521853616,1.51340940101261),.UNSPECIFIED.);
#214=B_SPLINE_CURVE_WITH_KNOTS('',3,(#8794,#8795,#8796,#8797,#8798,#8799,
#8800,#8801,#8802,#8803,#8804,#8805,#8806,#8807,#8808,#8809,#8810,#8811,
#8812,#8813,#8814,#8815,#8816,#8817,#8818,#8819,#8820,#8821,#8822,#8823,
#8824,#8825,#8826,#8827),.UNSPECIFIED.,.T.,.F.,(4,2,2,2,2,2,2,2,2,2,2,2,
2,2,2,2,4),(0.,0.0945941824764479,0.189188364952896,0.283770357603024,0.378352350253152,
0.47293434290328,0.567516335553408,0.662110518029856,0.756704700506303,
0.851298882982751,0.945893065459199,1.04047505810933,1.13505705075946,1.22963904340958,
1.32422103605971,1.41881521853616,1.51340940101261),.UNSPECIFIED.);
#215=B_SPLINE_CURVE_WITH_KNOTS('',3,(#9357,#9358,#9359,#9360,#9361,#9362,
#9363,#9364,#9365,#9366,#9367,#9368,#9369,#9370,#9371,#9372,#9373,#9374,
#9375,#9376,#9377,#9378),.UNSPECIFIED.,.F.,.F.,(4,2,2,2,2,2,2,2,2,2,4),
(0.0473477652366656,0.126350602536658,0.189525903804987,0.252701205073317,
0.313298422430275,0.373895639787233,0.434492857144191,0.495090074501149,
0.558265375769478,0.621440677037807,0.7004435143378),.UNSPECIFIED.);
#216=B_SPLINE_CURVE_WITH_KNOTS('',3,(#9382,#9383,#9384,#9385,#9386,#9387,
#9388,#9389,#9390,#9391,#9392,#9393,#9394,#9395,#9396,#9397,#9398,#9399,
#9400,#9401,#9402,#9403),.UNSPECIFIED.,.F.,.F.,(4,2,2,2,2,2,2,2,2,2,4),
(0.0464897534940957,0.0852567806515119,0.170513561303024,0.246687263103517,
0.308657850341199,0.370628437578881,0.432599024816563,0.494569612054245,
0.570743313854739,0.656000094506251,0.694767121663666),.UNSPECIFIED.);
#217=B_SPLINE_CURVE_WITH_KNOTS('',3,(#9409,#9410,#9411,#9412,#9413,#9414,
#9415,#9416,#9417,#9418,#9419,#9420,#9421,#9422,#9423,#9424,#9425,#9426,
#9427,#9428,#9429,#9430),.UNSPECIFIED.,.F.,.F.,(4,2,2,2,2,2,2,2,2,2,4),
(0.0464897534940957,0.0852567806515118,0.170513561303024,0.246687263103517,
0.308657850341199,0.370628437578881,0.432599024816563,0.494569612054245,
0.570743313854738,0.65600009450625,0.694767121663666),.UNSPECIFIED.);
#218=B_SPLINE_CURVE_WITH_KNOTS('',3,(#9434,#9435,#9436,#9437,#9438,#9439,
#9440,#9441,#9442,#9443,#9444,#9445,#9446,#9447,#9448,#9449,#9450,#9451,
#9452,#9453,#9454,#9455),.UNSPECIFIED.,.F.,.F.,(4,2,2,2,2,2,2,2,2,2,4),
(0.0464897534940957,0.0852567806515119,0.170513561303024,0.246687263103517,
0.308657850341199,0.370628437578881,0.432599024816563,0.494569612054245,
0.570743313854739,0.656000094506251,0.694767121663666),.UNSPECIFIED.);
#219=B_SPLINE_CURVE_WITH_KNOTS('',3,(#9459,#9460,#9461,#9462,#9463,#9464,
#9465,#9466,#9467,#9468,#9469,#9470),.UNSPECIFIED.,.F.,.F.,(4,2,2,2,2,4),
(0.0464897534940957,0.0852567806515119,0.170513561303024,0.246687263103517,
0.308657850341199,0.370628437578881),.UNSPECIFIED.);
#220=B_SPLINE_CURVE_WITH_KNOTS('',3,(#9475,#9476,#9477,#9478,#9479,#9480,
#9481,#9482,#9483,#9484,#9485,#9486),.UNSPECIFIED.,.F.,.F.,(4,2,2,2,2,4),
(0.370628437578881,0.432599024816563,0.494569612054245,0.570743313854738,
0.65600009450625,0.694767121663666),.UNSPECIFIED.);
#221=B_SPLINE_CURVE_WITH_KNOTS('',3,(#9490,#9491,#9492,#9493,#9494,#9495,
#9496,#9497,#9498,#9499,#9500,#9501,#9502,#9503,#9504,#9505,#9506,#9507,
#9508,#9509,#9510,#9511),.UNSPECIFIED.,.F.,.F.,(4,2,2,2,2,2,2,2,2,2,4),
(0.0464897534940957,0.0852567806515121,0.170513561303024,0.246687263103518,
0.308657850341199,0.370628437578881,0.432599024816563,0.494569612054245,
0.570743313854738,0.65600009450625,0.694767121663666),.UNSPECIFIED.);
#222=B_SPLINE_CURVE_WITH_KNOTS('',3,(#9515,#9516,#9517,#9518,#9519,#9520,
#9521,#9522,#9523,#9524,#9525,#9526,#9527,#9528,#9529,#9530,#9531,#9532,
#9533,#9534,#9535,#9536),.UNSPECIFIED.,.F.,.F.,(4,2,2,2,2,2,2,2,2,2,4),
(0.0464897534940957,0.0852567806515119,0.170513561303024,0.246687263103517,
0.308657850341199,0.370628437578881,0.432599024816563,0.494569612054245,
0.570743313854738,0.65600009450625,0.694767121663667),.UNSPECIFIED.);
#223=B_SPLINE_CURVE_WITH_KNOTS('',3,(#9540,#9541,#9542,#9543,#9544,#9545,
#9546,#9547,#9548,#9549,#9550,#9551,#9552,#9553,#9554,#9555,#9556,#9557,
#9558,#9559,#9560,#9561),.UNSPECIFIED.,.F.,.F.,(4,2,2,2,2,2,2,2,2,2,4),
(0.0464897534940957,0.0852567806515119,0.170513561303024,0.246687263103517,
0.308657850341199,0.370628437578881,0.432599024816563,0.494569612054245,
0.570743313854738,0.65600009450625,0.694767121663666),.UNSPECIFIED.);
#224=B_SPLINE_CURVE_WITH_KNOTS('',3,(#9565,#9566,#9567,#9568,#9569,#9570,
#9571,#9572,#9573,#9574,#9575,#9576,#9577,#9578,#9579,#9580,#9581,#9582,
#9583,#9584,#9585,#9586),.UNSPECIFIED.,.F.,.F.,(4,2,2,2,2,2,2,2,2,2,4),
(0.0464897534940957,0.0852567806515119,0.170513561303024,0.246687263103517,
0.308657850341199,0.370628437578881,0.432599024816563,0.494569612054245,
0.570743313854739,0.656000094506251,0.694767121663667),.UNSPECIFIED.);
#225=B_SPLINE_CURVE_WITH_KNOTS('',3,(#9594,#9595,#9596,#9597,#9598,#9599,
#9600,#9601,#9602,#9603,#9604,#9605,#9606,#9607,#9608,#9609,#9610,#9611,
#9612,#9613,#9614,#9615),.UNSPECIFIED.,.F.,.F.,(4,2,2,2,2,2,2,2,2,2,4),
(0.0473477652366656,0.126350602536658,0.189525903804987,0.252701205073316,
0.313298422430274,0.373895639787232,0.434492857144191,0.495090074501149,
0.558265375769478,0.621440677037807,0.7004435143378),.UNSPECIFIED.);
#226=B_SPLINE_CURVE_WITH_KNOTS('',3,(#9623,#9624,#9625,#9626,#9627,#9628,
#9629,#9630,#9631,#9632,#9633,#9634,#9635,#9636,#9637,#9638,#9639,#9640,
#9641,#9642,#9643,#9644),.UNSPECIFIED.,.F.,.F.,(4,2,2,2,2,2,2,2,2,2,4),
(0.0473477652366656,0.126350602536658,0.189525903804987,0.252701205073317,
0.313298422430275,0.373895639787233,0.434492857144191,0.495090074501149,
0.558265375769478,0.621440677037807,0.7004435143378),.UNSPECIFIED.);
#227=B_SPLINE_CURVE_WITH_KNOTS('',3,(#9653,#9654,#9655,#9656,#9657,#9658,
#9659,#9660,#9661,#9662,#9663,#9664),.UNSPECIFIED.,.F.,.F.,(4,2,2,2,2,4),
(0.0473477652366656,0.126350602536658,0.189525903804987,0.252701205073316,
0.313298422430275,0.373895639787233),.UNSPECIFIED.);
#228=B_SPLINE_CURVE_WITH_KNOTS('',3,(#9666,#9667,#9668,#9669,#9670,#9671,
#9672,#9673,#9674,#9675,#9676,#9677),.UNSPECIFIED.,.F.,.F.,(4,2,2,2,2,4),
(0.373895639787233,0.434492857144191,0.495090074501149,0.558265375769478,
0.621440677037807,0.7004435143378),.UNSPECIFIED.);
#229=B_SPLINE_CURVE_WITH_KNOTS('',3,(#9684,#9685,#9686,#9687,#9688,#9689,
#9690,#9691,#9692,#9693,#9694,#9695,#9696,#9697,#9698,#9699,#9700,#9701,
#9702,#9703,#9704,#9705),.UNSPECIFIED.,.F.,.F.,(4,2,2,2,2,2,2,2,2,2,4),
(0.0473477652366656,0.126350602536658,0.189525903804987,0.252701205073316,
0.313298422430275,0.373895639787233,0.434492857144191,0.495090074501149,
0.558265375769478,0.621440677037807,0.7004435143378),.UNSPECIFIED.);
#230=B_SPLINE_CURVE_WITH_KNOTS('',3,(#9713,#9714,#9715,#9716,#9717,#9718,
#9719,#9720,#9721,#9722,#9723,#9724,#9725,#9726,#9727,#9728,#9729,#9730,
#9731,#9732,#9733,#9734),.UNSPECIFIED.,.F.,.F.,(4,2,2,2,2,2,2,2,2,2,4),
(0.0473477652366656,0.126350602536658,0.189525903804987,0.252701205073317,
0.313298422430275,0.373895639787233,0.434492857144191,0.495090074501149,
0.558265375769478,0.621440677037807,0.7004435143378),.UNSPECIFIED.);
#231=B_SPLINE_CURVE_WITH_KNOTS('',3,(#9742,#9743,#9744,#9745,#9746,#9747,
#9748,#9749,#9750,#9751,#9752,#9753,#9754,#9755,#9756,#9757,#9758,#9759,
#9760,#9761,#9762,#9763),.UNSPECIFIED.,.F.,.F.,(4,2,2,2,2,2,2,2,2,2,4),
(0.0473477652366656,0.126350602536658,0.189525903804987,0.252701205073316,
0.313298422430275,0.373895639787233,0.434492857144191,0.495090074501149,
0.558265375769478,0.621440677037807,0.7004435143378),.UNSPECIFIED.);
#232=B_SPLINE_CURVE_WITH_KNOTS('',3,(#9772,#9773,#9774,#9775,#9776,#9777,
#9778,#9779,#9780,#9781,#9782,#9783,#9784,#9785,#9786,#9787,#9788,#9789,
#9790,#9791,#9792,#9793),.UNSPECIFIED.,.F.,.F.,(4,2,2,2,2,2,2,2,2,2,4),
(0.0473477652366656,0.126350602536658,0.189525903804987,0.252701205073317,
0.313298422430275,0.373895639787233,0.434492857144191,0.495090074501149,
0.558265375769478,0.621440677037807,0.7004435143378),.UNSPECIFIED.);
#233=B_SPLINE_CURVE_WITH_KNOTS('',3,(#9946,#9947,#9948,#9949,#9950,#9951,
#9952,#9953,#9954,#9955,#9956,#9957,#9958,#9959,#9960,#9961,#9962,#9963,
#9964,#9965,#9966,#9967,#9968,#9969,#9970,#9971,#9972,#9973,#9974,#9975,
#9976,#9977,#9978,#9979),.UNSPECIFIED.,.T.,.F.,(4,2,2,2,2,2,2,2,2,2,2,2,
2,2,2,2,4),(0.,0.0623062782223143,0.124612556444629,0.186916384615149,0.249220212785669,
0.31152404095619,0.37382786912671,0.436134147349024,0.498440425571339,0.560746703793653,
0.623052982015967,0.685356810186488,0.747660638357008,0.809964466527529,
0.872268294698049,0.934574572920363,0.996880851142677),.UNSPECIFIED.);
#234=B_SPLINE_CURVE_WITH_KNOTS('',3,(#9982,#9983,#9984,#9985,#9986,#9987,
#9988,#9989,#9990,#9991,#9992,#9993,#9994,#9995),.UNSPECIFIED.,.F.,.F.,
(4,2,2,2,2,2,4),(0.618551524396292,0.626563103102765,0.689203386094988,
0.751843669087211,0.814483952079434,0.877124235071657,0.88513581377813),
 .UNSPECIFIED.);
#235=B_SPLINE_CURVE_WITH_KNOTS('',3,(#9998,#9999,#10000,#10001,#10002,#10003,
#10004,#10005,#10006,#10007,#10008,#10009,#10010,#10011),.UNSPECIFIED.,
 .F.,.F.,(4,2,2,2,2,2,4),(0.117322411671485,0.125333990377958,0.187974273370181,
0.250614556362404,0.313254839354627,0.37589512234685,0.383906701053323),
 .UNSPECIFIED.);
#236=B_SPLINE_CURVE_WITH_KNOTS('',3,(#10022,#10023,#10024,#10025,#10026,
#10027,#10028,#10029,#10030,#10031),.UNSPECIFIED.,.F.,.F.,(4,2,2,2,4),(0.,
0.0623062782223142,0.124612556444628,0.186916384615149,0.249220212785669),
 .UNSPECIFIED.);
#237=B_SPLINE_CURVE_WITH_KNOTS('',3,(#10033,#10034,#10035,#10036,#10037,
#10038,#10039,#10040,#10041,#10042),.UNSPECIFIED.,.F.,.F.,(4,2,2,2,4),(0.747660638357008,
0.809964466527529,0.872268294698049,0.934574572920363,0.996880851142677),
 .UNSPECIFIED.);
#238=B_SPLINE_CURVE_WITH_KNOTS('',3,(#10043,#10044,#10045,#10046,#10047,
#10048,#10049,#10050,#10051,#10052,#10053,#10054,#10055,#10056,#10057,#10058,
#10059,#10060),.UNSPECIFIED.,.F.,.F.,(4,2,2,2,2,2,2,2,4),(0.249220212785669,
0.31152404095619,0.37382786912671,0.436134147349024,0.498440425571339,0.560746703793653,
0.623052982015967,0.685356810186488,0.747660638357008),.UNSPECIFIED.);
#239=B_SPLINE_CURVE_WITH_KNOTS('',3,(#10064,#10065,#10066,#10067,#10068,
#10069,#10070,#10071),.UNSPECIFIED.,.F.,.F.,(4,2,2,4),(0.618551524396292,
0.626563103102765,0.689203386094988,0.751843669087211),.UNSPECIFIED.);
#240=B_SPLINE_CURVE_WITH_KNOTS('',3,(#10075,#10076,#10077,#10078,#10079,
#10080,#10081,#10082),.UNSPECIFIED.,.F.,.F.,(4,2,2,4),(0.250614556362404,
0.313254839354627,0.37589512234685,0.383906701053323),.UNSPECIFIED.);
#241=B_SPLINE_CURVE_WITH_KNOTS('',3,(#10083,#10084,#10085,#10086,#10087,
#10088,#10089,#10090),.UNSPECIFIED.,.F.,.F.,(4,2,2,4),(0.117322411671484,
0.125333990377958,0.187974273370181,0.250614556362404),.UNSPECIFIED.);
#242=B_SPLINE_CURVE_WITH_KNOTS('',3,(#10091,#10092,#10093,#10094,#10095,
#10096,#10097,#10098),.UNSPECIFIED.,.F.,.F.,(4,2,2,4),(0.751843669087211,
0.814483952079434,0.877124235071657,0.885135813778131),.UNSPECIFIED.);
#243=B_SPLINE_CURVE_WITH_KNOTS('',3,(#10658,#10659,#10660,#10661,#10662,
#10663,#10664,#10665,#10666,#10667,#10668,#10669,#10670,#10671,#10672,#10673,
#10674,#10675,#10676,#10677,#10678,#10679,#10680,#10681,#10682,#10683,#10684,
#10685,#10686,#10687,#10688,#10689,#10690,#10691),.UNSPECIFIED.,.T.,.F.,
(4,2,2,2,2,2,2,2,2,2,2,2,2,2,2,2,4),(0.,0.0623062782223143,0.124612556444629,
0.186916384615149,0.249220212785669,0.31152404095619,0.37382786912671,0.436134147349024,
0.498440425571339,0.560746703793653,0.623052982015967,0.685356810186488,
0.747660638357008,0.809964466527529,0.872268294698049,0.934574572920363,
0.996880851142678),.UNSPECIFIED.);
#244=B_SPLINE_CURVE_WITH_KNOTS('',3,(#10694,#10695,#10696,#10697,#10698,
#10699,#10700,#10701,#10702,#10703,#10704,#10705,#10706,#10707),
 .UNSPECIFIED.,.F.,.F.,(4,2,2,2,2,2,4),(0.618551524396292,0.626563103102765,
0.689203386094988,0.751843669087211,0.814483952079434,0.877124235071657,
0.88513581377813),.UNSPECIFIED.);
#245=B_SPLINE_CURVE_WITH_KNOTS('',3,(#10710,#10711,#10712,#10713,#10714,
#10715,#10716,#10717,#10718,#10719,#10720,#10721,#10722,#10723),
 .UNSPECIFIED.,.F.,.F.,(4,2,2,2,2,2,4),(0.117322411671484,0.125333990377958,
0.187974273370181,0.250614556362404,0.313254839354627,0.37589512234685,
0.383906701053322),.UNSPECIFIED.);
#246=B_SPLINE_CURVE_WITH_KNOTS('',3,(#10734,#10735,#10736,#10737,#10738,
#10739,#10740,#10741,#10742,#10743),.UNSPECIFIED.,.F.,.F.,(4,2,2,2,4),(0.,
0.0623062782223142,0.124612556444628,0.186916384615149,0.249220212785669),
 .UNSPECIFIED.);
#247=B_SPLINE_CURVE_WITH_KNOTS('',3,(#10745,#10746,#10747,#10748,#10749,
#10750,#10751,#10752,#10753,#10754),.UNSPECIFIED.,.F.,.F.,(4,2,2,2,4),(0.747660638357008,
0.809964466527528,0.872268294698049,0.934574572920363,0.996880851142677),
 .UNSPECIFIED.);
#248=B_SPLINE_CURVE_WITH_KNOTS('',3,(#10755,#10756,#10757,#10758,#10759,
#10760,#10761,#10762,#10763,#10764,#10765,#10766,#10767,#10768,#10769,#10770,
#10771,#10772),.UNSPECIFIED.,.F.,.F.,(4,2,2,2,2,2,2,2,4),(0.249220212785669,
0.31152404095619,0.37382786912671,0.436134147349024,0.498440425571339,0.560746703793653,
0.623052982015967,0.685356810186488,0.747660638357008),.UNSPECIFIED.);
#249=B_SPLINE_CURVE_WITH_KNOTS('',3,(#10776,#10777,#10778,#10779,#10780,
#10781,#10782,#10783),.UNSPECIFIED.,.F.,.F.,(4,2,2,4),(0.618551507245623,
0.626563103102765,0.689203386094988,0.751843669087211),.UNSPECIFIED.);
#250=B_SPLINE_CURVE_WITH_KNOTS('',3,(#10787,#10788,#10789,#10790,#10791,
#10792,#10793,#10794),.UNSPECIFIED.,.F.,.F.,(4,2,2,4),(0.250614556362404,
0.313254839354627,0.37589512234685,0.383906718203992),.UNSPECIFIED.);
#251=B_SPLINE_CURVE_WITH_KNOTS('',3,(#10795,#10796,#10797,#10798,#10799,
#10800,#10801,#10802),.UNSPECIFIED.,.F.,.F.,(4,2,2,4),(0.117322394520816,
0.125333990377958,0.187974273370181,0.250614556362404),.UNSPECIFIED.);
#252=B_SPLINE_CURVE_WITH_KNOTS('',3,(#10803,#10804,#10805,#10806,#10807,
#10808,#10809,#10810),.UNSPECIFIED.,.F.,.F.,(4,2,2,4),(0.751843669087211,
0.814483952079434,0.877124235071657,0.8851358309288),.UNSPECIFIED.);
#253=SHAPE_REPRESENTATION_RELATIONSHIP('SRR','None',#11066,#278);
#254=SHAPE_REPRESENTATION_RELATIONSHIP('SRR','None',#11067,#279);
#255=SHAPE_REPRESENTATION_RELATIONSHIP('SRR','None',#11068,#280);
#256=SHAPE_REPRESENTATION_RELATIONSHIP('SRR','None',#11069,#281);
#257=SHAPE_REPRESENTATION_RELATIONSHIP('SRR','None',#11070,#282);
#258=SHAPE_REPRESENTATION_RELATIONSHIP('SRR','None',#11071,#283);
#259=SHAPE_REPRESENTATION_RELATIONSHIP('SRR','None',#11072,#284);
#260=SHAPE_REPRESENTATION_RELATIONSHIP('SRR','None',#11074,#285);
#261=SHAPE_REPRESENTATION_RELATIONSHIP('SRR','None',#11075,#286);
#262=SHAPE_REPRESENTATION_RELATIONSHIP('SRR','None',#11076,#287);
#263=SHAPE_REPRESENTATION_RELATIONSHIP('SRR','None',#11077,#288);
#264=SHAPE_REPRESENTATION_RELATIONSHIP('SRR','None',#11078,#289);
#265=SHAPE_REPRESENTATION_RELATIONSHIP('SRR','None',#11080,#290);
#266=SHAPE_REPRESENTATION_RELATIONSHIP('SRR','None',#11081,#291);
#267=SHAPE_REPRESENTATION_RELATIONSHIP('SRR','None',#11082,#292);
#268=SHAPE_REPRESENTATION_RELATIONSHIP('SRR','None',#11083,#293);
#269=SHAPE_REPRESENTATION_RELATIONSHIP('SRR','None',#11084,#294);
#270=SHAPE_REPRESENTATION_RELATIONSHIP('SRR','None',#11085,#295);
#271=SHAPE_REPRESENTATION_RELATIONSHIP('SRR','None',#11086,#296);
#272=SHAPE_REPRESENTATION_RELATIONSHIP('SRR','None',#11087,#297);
#273=SHAPE_REPRESENTATION_RELATIONSHIP('SRR','None',#11088,#298);
#274=SHAPE_REPRESENTATION_RELATIONSHIP('SRR','None',#11090,#299);
#275=SHAPE_REPRESENTATION_RELATIONSHIP('SRR','None',#11091,#300);
#276=SHAPE_REPRESENTATION_RELATIONSHIP('SRR','None',#11092,#301);
#277=SHAPE_REPRESENTATION_RELATIONSHIP('SRR','None',#11093,#302);
#278=ADVANCED_BREP_SHAPE_REPRESENTATION('',(#336),#10929);
#279=ADVANCED_BREP_SHAPE_REPRESENTATION('',(#337),#10930);
#280=ADVANCED_BREP_SHAPE_REPRESENTATION('',(#338),#10931);
#281=ADVANCED_BREP_SHAPE_REPRESENTATION('',(#339),#10932);
#282=ADVANCED_BREP_SHAPE_REPRESENTATION('',(#340),#10933);
#283=ADVANCED_BREP_SHAPE_REPRESENTATION('',(#341),#10934);
#284=ADVANCED_BREP_SHAPE_REPRESENTATION('',(#211),#10935);
#285=ADVANCED_BREP_SHAPE_REPRESENTATION('',(#342),#10937);
#286=ADVANCED_BREP_SHAPE_REPRESENTATION('',(#343),#10938);
#287=ADVANCED_BREP_SHAPE_REPRESENTATION('',(#344,#345,#346,#347,#348,#349,
#350,#351),#10939);
#288=ADVANCED_BREP_SHAPE_REPRESENTATION('',(#352),#10940);
#289=ADVANCED_BREP_SHAPE_REPRESENTATION('',(#353,#354),#10941);
#290=ADVANCED_BREP_SHAPE_REPRESENTATION('',(#355),#10943);
#291=ADVANCED_BREP_SHAPE_REPRESENTATION('',(#356),#10944);
#292=ADVANCED_BREP_SHAPE_REPRESENTATION('',(#357),#10945);
#293=ADVANCED_BREP_SHAPE_REPRESENTATION('',(#358),#10946);
#294=ADVANCED_BREP_SHAPE_REPRESENTATION('',(#359),#10947);
#295=ADVANCED_BREP_SHAPE_REPRESENTATION('',(#360),#10948);
#296=ADVANCED_BREP_SHAPE_REPRESENTATION('',(#361),#10949);
#297=ADVANCED_BREP_SHAPE_REPRESENTATION('',(#362),#10950);
#298=ADVANCED_BREP_SHAPE_REPRESENTATION('',(#212),#10951);
#299=ADVANCED_BREP_SHAPE_REPRESENTATION('',(#363),#10953);
#300=ADVANCED_BREP_SHAPE_REPRESENTATION('',(#364),#10954);
#301=ADVANCED_BREP_SHAPE_REPRESENTATION('',(#365),#10955);
#302=ADVANCED_BREP_SHAPE_REPRESENTATION('',(#366),#10956);
#303=STYLED_ITEM('',(#11266),#336);
#304=STYLED_ITEM('',(#11273),#337);
#305=STYLED_ITEM('',(#11273),#338);
#306=STYLED_ITEM('',(#11287),#339);
#307=STYLED_ITEM('',(#11287),#340);
#308=STYLED_ITEM('',(#11287),#341);
#309=STYLED_ITEM('',(#11294),#211);
#310=STYLED_ITEM('',(#11287),#342);
#311=STYLED_ITEM('',(#11287),#343);
#312=STYLED_ITEM('',(#11287),#344);
#313=STYLED_ITEM('',(#11287),#345);
#314=STYLED_ITEM('',(#11287),#346);
#315=STYLED_ITEM('',(#11287),#347);
#316=STYLED_ITEM('',(#11287),#348);
#317=STYLED_ITEM('',(#11287),#349);
#318=STYLED_ITEM('',(#11287),#350);
#319=STYLED_ITEM('',(#11287),#351);
#320=STYLED_ITEM('',(#11287),#352);
#321=STYLED_ITEM('',(#11287),#353);
#322=STYLED_ITEM('',(#11287),#354);
#323=STYLED_ITEM('',(#11280),#355);
#324=STYLED_ITEM('',(#11287),#356);
#325=STYLED_ITEM('',(#11301),#357);
#326=STYLED_ITEM('',(#11287),#358);
#327=STYLED_ITEM('',(#11280),#359);
#328=STYLED_ITEM('',(#11301),#360);
#329=STYLED_ITEM('',(#11273),#361);
#330=STYLED_ITEM('',(#11294),#362);
#331=STYLED_ITEM('',(#11294),#212);
#332=STYLED_ITEM('',(#11280),#363);
#333=STYLED_ITEM('',(#11287),#364);
#334=STYLED_ITEM('',(#11301),#365);
#335=STYLED_ITEM('',(#11294),#366);
#336=MANIFOLD_SOLID_BREP('Body1',#5699);
#337=MANIFOLD_SOLID_BREP('Body1',#5700);
#338=MANIFOLD_SOLID_BREP('Body1',#5701);
#339=MANIFOLD_SOLID_BREP('Body1',#5702);
#340=MANIFOLD_SOLID_BREP('Body1',#5703);
#341=MANIFOLD_SOLID_BREP('Body1',#5704);
#342=MANIFOLD_SOLID_BREP('Body1',#5707);
#343=MANIFOLD_SOLID_BREP('Body1',#5708);
#344=MANIFOLD_SOLID_BREP('Body1',#5709);
#345=MANIFOLD_SOLID_BREP('Body2',#5710);
#346=MANIFOLD_SOLID_BREP('Body3',#5711);
#347=MANIFOLD_SOLID_BREP('Body4',#5712);
#348=MANIFOLD_SOLID_BREP('Body5',#5713);
#349=MANIFOLD_SOLID_BREP('Body6',#5714);
#350=MANIFOLD_SOLID_BREP('Body7',#5715);
#351=MANIFOLD_SOLID_BREP('Body8',#5716);
#352=MANIFOLD_SOLID_BREP('Continuous crown cage',#5717);
#353=MANIFOLD_SOLID_BREP('Body1',#5718);
#354=MANIFOLD_SOLID_BREP('Body2',#5719);
#355=MANIFOLD_SOLID_BREP('Body1',#5720);
#356=MANIFOLD_SOLID_BREP('Body1',#5721);
#357=MANIFOLD_SOLID_BREP('Body1',#5722);
#358=MANIFOLD_SOLID_BREP('Body1',#5723);
#359=MANIFOLD_SOLID_BREP('Body1',#5724);
#360=MANIFOLD_SOLID_BREP('Body1',#5725);
#361=MANIFOLD_SOLID_BREP('Body1',#5726);
#362=MANIFOLD_SOLID_BREP('Body1',#5727);
#363=MANIFOLD_SOLID_BREP('Body1',#5730);
#364=MANIFOLD_SOLID_BREP('Body1',#5731);
#365=MANIFOLD_SOLID_BREP('Body1',#5732);
#366=MANIFOLD_SOLID_BREP('Body1',#5733);
#367=FACE_BOUND('',#994,.T.);
#368=FACE_BOUND('',#995,.T.);
#369=FACE_BOUND('',#996,.T.);
#370=FACE_BOUND('',#997,.T.);
#371=FACE_BOUND('',#999,.T.);
#372=FACE_BOUND('',#1000,.T.);
#373=FACE_BOUND('',#1001,.T.);
#374=FACE_BOUND('',#1002,.T.);
#375=FACE_BOUND('',#1026,.T.);
#376=FACE_BOUND('',#1028,.T.);
#377=FACE_BOUND('',#1040,.T.);
#378=FACE_BOUND('',#1042,.T.);
#379=FACE_BOUND('',#1046,.T.);
#380=FACE_BOUND('',#1050,.T.);
#381=FACE_BOUND('',#1054,.T.);
#382=FACE_BOUND('',#1058,.T.);
#383=FACE_BOUND('',#1063,.T.);
#384=FACE_BOUND('',#1064,.T.);
#385=FACE_BOUND('',#1065,.T.);
#386=FACE_BOUND('',#1066,.T.);
#387=FACE_BOUND('',#1067,.T.);
#388=FACE_BOUND('',#1068,.T.);
#389=FACE_BOUND('',#1069,.T.);
#390=FACE_BOUND('',#1070,.T.);
#391=FACE_BOUND('',#1071,.T.);
#392=FACE_BOUND('',#1072,.T.);
#393=FACE_BOUND('',#1081,.T.);
#394=FACE_BOUND('',#1082,.T.);
#395=FACE_BOUND('',#1085,.T.);
#396=FACE_BOUND('',#1086,.T.);
#397=FACE_BOUND('',#1087,.T.);
#398=FACE_BOUND('',#1088,.T.);
#399=FACE_BOUND('',#1089,.T.);
#400=FACE_BOUND('',#1090,.T.);
#401=FACE_BOUND('',#1093,.T.);
#402=FACE_BOUND('',#1095,.T.);
#403=FACE_BOUND('',#1098,.T.);
#404=FACE_BOUND('',#1101,.T.);
#405=FACE_BOUND('',#1104,.T.);
#406=FACE_BOUND('',#1111,.T.);
#407=FACE_BOUND('',#1115,.T.);
#408=FACE_BOUND('',#1116,.T.);
#409=FACE_BOUND('',#1117,.T.);
#410=FACE_BOUND('',#1118,.T.);
#411=FACE_BOUND('',#1119,.T.);
#412=FACE_BOUND('',#1122,.T.);
#413=FACE_BOUND('',#1124,.T.);
#414=FACE_BOUND('',#1127,.T.);
#415=FACE_BOUND('',#1130,.T.);
#416=FACE_BOUND('',#1133,.T.);
#417=FACE_BOUND('',#1140,.T.);
#418=FACE_BOUND('',#1144,.T.);
#419=FACE_BOUND('',#1145,.T.);
#420=FACE_BOUND('',#1146,.T.);
#421=FACE_BOUND('',#1147,.T.);
#422=FACE_BOUND('',#1148,.T.);
#423=FACE_BOUND('',#1154,.T.);
#424=FACE_BOUND('',#1172,.T.);
#425=FACE_BOUND('',#1175,.T.);
#426=FACE_BOUND('',#1180,.T.);
#427=FACE_BOUND('',#1185,.T.);
#428=FACE_BOUND('',#1213,.T.);
#429=FACE_BOUND('',#1216,.T.);
#430=FACE_BOUND('',#1219,.T.);
#431=FACE_BOUND('',#1222,.T.);
#432=FACE_BOUND('',#1225,.T.);
#433=FACE_BOUND('',#1232,.T.);
#434=FACE_BOUND('',#1233,.T.);
#435=FACE_BOUND('',#1240,.T.);
#436=FACE_BOUND('',#1241,.T.);
#437=FACE_BOUND('',#1245,.T.);
#438=FACE_BOUND('',#1250,.T.);
#439=FACE_BOUND('',#1255,.T.);
#440=FACE_BOUND('',#1257,.T.);
#441=FACE_BOUND('',#1265,.T.);
#442=FACE_BOUND('',#1267,.T.);
#443=FACE_BOUND('',#1269,.T.);
#444=FACE_BOUND('',#1271,.T.);
#445=FACE_BOUND('',#1273,.T.);
#446=FACE_BOUND('',#1275,.T.);
#447=FACE_BOUND('',#1284,.T.);
#448=FACE_BOUND('',#1289,.T.);
#449=FACE_BOUND('',#1293,.T.);
#450=FACE_BOUND('',#1295,.T.);
#451=FACE_BOUND('',#1299,.T.);
#452=FACE_BOUND('',#1301,.T.);
#453=FACE_BOUND('',#1305,.T.);
#454=FACE_BOUND('',#1307,.T.);
#455=FACE_BOUND('',#1322,.T.);
#456=FACE_BOUND('',#1337,.T.);
#457=FACE_BOUND('',#1338,.T.);
#458=FACE_BOUND('',#1339,.T.);
#459=FACE_BOUND('',#1340,.T.);
#460=FACE_BOUND('',#1349,.T.);
#461=FACE_BOUND('',#1351,.T.);
#462=FACE_BOUND('',#1363,.T.);
#463=FACE_BOUND('',#1374,.T.);
#464=FACE_BOUND('',#1388,.T.);
#465=FACE_BOUND('',#1394,.T.);
#466=FACE_BOUND('',#1396,.T.);
#467=FACE_BOUND('',#1404,.T.);
#468=FACE_BOUND('',#1406,.T.);
#469=FACE_BOUND('',#1408,.T.);
#470=FACE_BOUND('',#1410,.T.);
#471=FACE_BOUND('',#1420,.T.);
#472=PLANE('',#6025);
#473=PLANE('',#6026);
#474=PLANE('',#6027);
#475=PLANE('',#6028);
#476=PLANE('',#6029);
#477=PLANE('',#6030);
#478=PLANE('',#6032);
#479=PLANE('',#6033);
#480=PLANE('',#6034);
#481=PLANE('',#6035);
#482=PLANE('',#6036);
#483=PLANE('',#6037);
#484=PLANE('',#6039);
#485=PLANE('',#6040);
#486=PLANE('',#6041);
#487=PLANE('',#6042);
#488=PLANE('',#6043);
#489=PLANE('',#6044);
#490=PLANE('',#6051);
#491=PLANE('',#6055);
#492=PLANE('',#6059);
#493=PLANE('',#6063);
#494=PLANE('',#6067);
#495=PLANE('',#6076);
#496=PLANE('',#6080);
#497=PLANE('',#6084);
#498=PLANE('',#6088);
#499=PLANE('',#6092);
#500=PLANE('',#6102);
#501=PLANE('',#6110);
#502=PLANE('',#6118);
#503=PLANE('',#6126);
#504=PLANE('',#6128);
#505=PLANE('',#6129);
#506=PLANE('',#6130);
#507=PLANE('',#6131);
#508=PLANE('',#6132);
#509=PLANE('',#6141);
#510=PLANE('',#6142);
#511=PLANE('',#6143);
#512=PLANE('',#6144);
#513=PLANE('',#6145);
#514=PLANE('',#6150);
#515=PLANE('',#6154);
#516=PLANE('',#6160);
#517=PLANE('',#6166);
#518=PLANE('',#6172);
#519=PLANE('',#6189);
#520=PLANE('',#6194);
#521=PLANE('',#6199);
#522=PLANE('',#6203);
#523=PLANE('',#6209);
#524=PLANE('',#6215);
#525=PLANE('',#6221);
#526=PLANE('',#6238);
#527=PLANE('',#6243);
#528=PLANE('',#6245);
#529=PLANE('',#6253);
#530=PLANE('',#6261);
#531=PLANE('',#6262);
#532=PLANE('',#6263);
#533=PLANE('',#6264);
#534=PLANE('',#6265);
#535=PLANE('',#6266);
#536=PLANE('',#6267);
#537=PLANE('',#6268);
#538=PLANE('',#6269);
#539=PLANE('',#6285);
#540=PLANE('',#6288);
#541=PLANE('',#6300);
#542=PLANE('',#6309);
#543=PLANE('',#6342);
#544=PLANE('',#6347);
#545=PLANE('',#6352);
#546=PLANE('',#6357);
#547=PLANE('',#6362);
#548=PLANE('',#6367);
#549=PLANE('',#6376);
#550=PLANE('',#6380);
#551=PLANE('',#6381);
#552=PLANE('',#6383);
#553=PLANE('',#6388);
#554=PLANE('',#6391);
#555=PLANE('',#6396);
#556=PLANE('',#6409);
#557=PLANE('',#6416);
#558=PLANE('',#6420);
#559=PLANE('',#6421);
#560=PLANE('',#6422);
#561=PLANE('',#6423);
#562=PLANE('',#6424);
#563=PLANE('',#6425);
#564=PLANE('',#6431);
#565=PLANE('',#6439);
#566=PLANE('',#6440);
#567=PLANE('',#6448);
#568=PLANE('',#6449);
#569=PLANE('',#6451);
#570=PLANE('',#6456);
#571=PLANE('',#6457);
#572=PLANE('',#6461);
#573=PLANE('',#6468);
#574=PLANE('',#6469);
#575=PLANE('',#6471);
#576=PLANE('',#6474);
#577=PLANE('',#6482);
#578=PLANE('',#6483);
#579=PLANE('',#6491);
#580=PLANE('',#6493);
#581=PLANE('',#6494);
#582=PLANE('',#6497);
#583=PLANE('',#6505);
#584=PLANE('',#6506);
#585=PLANE('',#6514);
#586=PLANE('',#6515);
#587=PLANE('',#6523);
#588=PLANE('',#6524);
#589=PLANE('',#6526);
#590=PLANE('',#6527);
#591=PLANE('',#6528);
#592=PLANE('',#6529);
#593=PLANE('',#6530);
#594=PLANE('',#6531);
#595=PLANE('',#6532);
#596=PLANE('',#6533);
#597=PLANE('',#6534);
#598=PLANE('',#6536);
#599=PLANE('',#6544);
#600=PLANE('',#6604);
#601=PLANE('',#6618);
#602=PLANE('',#6619);
#603=PLANE('',#6620);
#604=PLANE('',#6621);
#605=PLANE('',#6622);
#606=PLANE('',#6623);
#607=PLANE('',#6628);
#608=PLANE('',#6632);
#609=PLANE('',#6644);
#610=PLANE('',#6646);
#611=PLANE('',#6647);
#612=PLANE('',#6648);
#613=PLANE('',#6649);
#614=PLANE('',#6650);
#615=PLANE('',#6651);
#616=PLANE('',#6655);
#617=PLANE('',#6658);
#618=PLANE('',#6660);
#619=PLANE('',#6661);
#620=PLANE('',#6662);
#621=PLANE('',#6663);
#622=PLANE('',#6664);
#623=PLANE('',#6665);
#624=PLANE('',#6669);
#625=PLANE('',#6672);
#626=PLANE('',#6674);
#627=PLANE('',#6675);
#628=PLANE('',#6676);
#629=PLANE('',#6677);
#630=PLANE('',#6678);
#631=PLANE('',#6681);
#632=PLANE('',#6682);
#633=PLANE('',#6683);
#634=PLANE('',#6687);
#635=PLANE('',#6695);
#636=PLANE('',#6696);
#637=PLANE('',#6698);
#638=PLANE('',#6703);
#639=PLANE('',#6704);
#640=PLANE('',#6708);
#641=PLANE('',#6715);
#642=PLANE('',#6716);
#643=PLANE('',#6718);
#644=PLANE('',#6720);
#645=PLANE('',#6721);
#646=PLANE('',#6722);
#647=PLANE('',#6723);
#648=PLANE('',#6724);
#649=PLANE('',#6725);
#650=PLANE('',#6726);
#651=PLANE('',#6727);
#652=FACE_OUTER_BOUND('',#985,.T.);
#653=FACE_OUTER_BOUND('',#986,.T.);
#654=FACE_OUTER_BOUND('',#987,.T.);
#655=FACE_OUTER_BOUND('',#988,.T.);
#656=FACE_OUTER_BOUND('',#989,.T.);
#657=FACE_OUTER_BOUND('',#990,.T.);
#658=FACE_OUTER_BOUND('',#991,.T.);
#659=FACE_OUTER_BOUND('',#992,.T.);
#660=FACE_OUTER_BOUND('',#993,.T.);
#661=FACE_OUTER_BOUND('',#998,.T.);
#662=FACE_OUTER_BOUND('',#1003,.T.);
#663=FACE_OUTER_BOUND('',#1004,.T.);
#664=FACE_OUTER_BOUND('',#1005,.T.);
#665=FACE_OUTER_BOUND('',#1006,.T.);
#666=FACE_OUTER_BOUND('',#1007,.T.);
#667=FACE_OUTER_BOUND('',#1008,.T.);
#668=FACE_OUTER_BOUND('',#1009,.T.);
#669=FACE_OUTER_BOUND('',#1010,.T.);
#670=FACE_OUTER_BOUND('',#1011,.T.);
#671=FACE_OUTER_BOUND('',#1012,.T.);
#672=FACE_OUTER_BOUND('',#1013,.T.);
#673=FACE_OUTER_BOUND('',#1014,.T.);
#674=FACE_OUTER_BOUND('',#1015,.T.);
#675=FACE_OUTER_BOUND('',#1016,.T.);
#676=FACE_OUTER_BOUND('',#1017,.T.);
#677=FACE_OUTER_BOUND('',#1018,.T.);
#678=FACE_OUTER_BOUND('',#1019,.T.);
#679=FACE_OUTER_BOUND('',#1020,.T.);
#680=FACE_OUTER_BOUND('',#1021,.T.);
#681=FACE_OUTER_BOUND('',#1022,.T.);
#682=FACE_OUTER_BOUND('',#1023,.T.);
#683=FACE_OUTER_BOUND('',#1024,.T.);
#684=FACE_OUTER_BOUND('',#1025,.T.);
#685=FACE_OUTER_BOUND('',#1027,.T.);
#686=FACE_OUTER_BOUND('',#1029,.T.);
#687=FACE_OUTER_BOUND('',#1030,.T.);
#688=FACE_OUTER_BOUND('',#1031,.T.);
#689=FACE_OUTER_BOUND('',#1032,.T.);
#690=FACE_OUTER_BOUND('',#1033,.T.);
#691=FACE_OUTER_BOUND('',#1034,.T.);
#692=FACE_OUTER_BOUND('',#1035,.T.);
#693=FACE_OUTER_BOUND('',#1036,.T.);
#694=FACE_OUTER_BOUND('',#1037,.T.);
#695=FACE_OUTER_BOUND('',#1038,.T.);
#696=FACE_OUTER_BOUND('',#1039,.T.);
#697=FACE_OUTER_BOUND('',#1041,.T.);
#698=FACE_OUTER_BOUND('',#1043,.T.);
#699=FACE_OUTER_BOUND('',#1044,.T.);
#700=FACE_OUTER_BOUND('',#1045,.T.);
#701=FACE_OUTER_BOUND('',#1047,.T.);
#702=FACE_OUTER_BOUND('',#1048,.T.);
#703=FACE_OUTER_BOUND('',#1049,.T.);
#704=FACE_OUTER_BOUND('',#1051,.T.);
#705=FACE_OUTER_BOUND('',#1052,.T.);
#706=FACE_OUTER_BOUND('',#1053,.T.);
#707=FACE_OUTER_BOUND('',#1055,.T.);
#708=FACE_OUTER_BOUND('',#1056,.T.);
#709=FACE_OUTER_BOUND('',#1057,.T.);
#710=FACE_OUTER_BOUND('',#1059,.T.);
#711=FACE_OUTER_BOUND('',#1060,.T.);
#712=FACE_OUTER_BOUND('',#1061,.T.);
#713=FACE_OUTER_BOUND('',#1062,.T.);
#714=FACE_OUTER_BOUND('',#1073,.T.);
#715=FACE_OUTER_BOUND('',#1074,.T.);
#716=FACE_OUTER_BOUND('',#1075,.T.);
#717=FACE_OUTER_BOUND('',#1076,.T.);
#718=FACE_OUTER_BOUND('',#1077,.T.);
#719=FACE_OUTER_BOUND('',#1078,.T.);
#720=FACE_OUTER_BOUND('',#1079,.T.);
#721=FACE_OUTER_BOUND('',#1080,.T.);
#722=FACE_OUTER_BOUND('',#1083,.T.);
#723=FACE_OUTER_BOUND('',#1084,.T.);
#724=FACE_OUTER_BOUND('',#1091,.T.);
#725=FACE_OUTER_BOUND('',#1092,.T.);
#726=FACE_OUTER_BOUND('',#1094,.T.);
#727=FACE_OUTER_BOUND('',#1096,.T.);
#728=FACE_OUTER_BOUND('',#1097,.T.);
#729=FACE_OUTER_BOUND('',#1099,.T.);
#730=FACE_OUTER_BOUND('',#1100,.T.);
#731=FACE_OUTER_BOUND('',#1102,.T.);
#732=FACE_OUTER_BOUND('',#1103,.T.);
#733=FACE_OUTER_BOUND('',#1105,.T.);
#734=FACE_OUTER_BOUND('',#1106,.T.);
#735=FACE_OUTER_BOUND('',#1107,.T.);
#736=FACE_OUTER_BOUND('',#1108,.T.);
#737=FACE_OUTER_BOUND('',#1109,.T.);
#738=FACE_OUTER_BOUND('',#1110,.T.);
#739=FACE_OUTER_BOUND('',#1112,.T.);
#740=FACE_OUTER_BOUND('',#1113,.T.);
#741=FACE_OUTER_BOUND('',#1114,.T.);
#742=FACE_OUTER_BOUND('',#1120,.T.);
#743=FACE_OUTER_BOUND('',#1121,.T.);
#744=FACE_OUTER_BOUND('',#1123,.T.);
#745=FACE_OUTER_BOUND('',#1125,.T.);
#746=FACE_OUTER_BOUND('',#1126,.T.);
#747=FACE_OUTER_BOUND('',#1128,.T.);
#748=FACE_OUTER_BOUND('',#1129,.T.);
#749=FACE_OUTER_BOUND('',#1131,.T.);
#750=FACE_OUTER_BOUND('',#1132,.T.);
#751=FACE_OUTER_BOUND('',#1134,.T.);
#752=FACE_OUTER_BOUND('',#1135,.T.);
#753=FACE_OUTER_BOUND('',#1136,.T.);
#754=FACE_OUTER_BOUND('',#1137,.T.);
#755=FACE_OUTER_BOUND('',#1138,.T.);
#756=FACE_OUTER_BOUND('',#1139,.T.);
#757=FACE_OUTER_BOUND('',#1141,.T.);
#758=FACE_OUTER_BOUND('',#1142,.T.);
#759=FACE_OUTER_BOUND('',#1143,.T.);
#760=FACE_OUTER_BOUND('',#1149,.T.);
#761=FACE_OUTER_BOUND('',#1150,.T.);
#762=FACE_OUTER_BOUND('',#1151,.T.);
#763=FACE_OUTER_BOUND('',#1152,.T.);
#764=FACE_OUTER_BOUND('',#1153,.T.);
#765=FACE_OUTER_BOUND('',#1155,.T.);
#766=FACE_OUTER_BOUND('',#1156,.T.);
#767=FACE_OUTER_BOUND('',#1157,.T.);
#768=FACE_OUTER_BOUND('',#1158,.T.);
#769=FACE_OUTER_BOUND('',#1159,.T.);
#770=FACE_OUTER_BOUND('',#1160,.T.);
#771=FACE_OUTER_BOUND('',#1161,.T.);
#772=FACE_OUTER_BOUND('',#1162,.T.);
#773=FACE_OUTER_BOUND('',#1163,.T.);
#774=FACE_OUTER_BOUND('',#1164,.T.);
#775=FACE_OUTER_BOUND('',#1165,.T.);
#776=FACE_OUTER_BOUND('',#1166,.T.);
#777=FACE_OUTER_BOUND('',#1167,.T.);
#778=FACE_OUTER_BOUND('',#1168,.T.);
#779=FACE_OUTER_BOUND('',#1169,.T.);
#780=FACE_OUTER_BOUND('',#1170,.T.);
#781=FACE_OUTER_BOUND('',#1171,.T.);
#782=FACE_OUTER_BOUND('',#1173,.T.);
#783=FACE_OUTER_BOUND('',#1174,.T.);
#784=FACE_OUTER_BOUND('',#1176,.T.);
#785=FACE_OUTER_BOUND('',#1177,.T.);
#786=FACE_OUTER_BOUND('',#1178,.T.);
#787=FACE_OUTER_BOUND('',#1179,.T.);
#788=FACE_OUTER_BOUND('',#1181,.T.);
#789=FACE_OUTER_BOUND('',#1182,.T.);
#790=FACE_OUTER_BOUND('',#1183,.T.);
#791=FACE_OUTER_BOUND('',#1184,.T.);
#792=FACE_OUTER_BOUND('',#1186,.T.);
#793=FACE_OUTER_BOUND('',#1187,.T.);
#794=FACE_OUTER_BOUND('',#1188,.T.);
#795=FACE_OUTER_BOUND('',#1189,.T.);
#796=FACE_OUTER_BOUND('',#1190,.T.);
#797=FACE_OUTER_BOUND('',#1191,.T.);
#798=FACE_OUTER_BOUND('',#1192,.T.);
#799=FACE_OUTER_BOUND('',#1193,.T.);
#800=FACE_OUTER_BOUND('',#1194,.T.);
#801=FACE_OUTER_BOUND('',#1195,.T.);
#802=FACE_OUTER_BOUND('',#1196,.T.);
#803=FACE_OUTER_BOUND('',#1197,.T.);
#804=FACE_OUTER_BOUND('',#1198,.T.);
#805=FACE_OUTER_BOUND('',#1199,.T.);
#806=FACE_OUTER_BOUND('',#1200,.T.);
#807=FACE_OUTER_BOUND('',#1201,.T.);
#808=FACE_OUTER_BOUND('',#1202,.T.);
#809=FACE_OUTER_BOUND('',#1203,.T.);
#810=FACE_OUTER_BOUND('',#1204,.T.);
#811=FACE_OUTER_BOUND('',#1205,.T.);
#812=FACE_OUTER_BOUND('',#1206,.T.);
#813=FACE_OUTER_BOUND('',#1207,.T.);
#814=FACE_OUTER_BOUND('',#1208,.T.);
#815=FACE_OUTER_BOUND('',#1209,.T.);
#816=FACE_OUTER_BOUND('',#1210,.T.);
#817=FACE_OUTER_BOUND('',#1211,.T.);
#818=FACE_OUTER_BOUND('',#1212,.T.);
#819=FACE_OUTER_BOUND('',#1214,.T.);
#820=FACE_OUTER_BOUND('',#1215,.T.);
#821=FACE_OUTER_BOUND('',#1217,.T.);
#822=FACE_OUTER_BOUND('',#1218,.T.);
#823=FACE_OUTER_BOUND('',#1220,.T.);
#824=FACE_OUTER_BOUND('',#1221,.T.);
#825=FACE_OUTER_BOUND('',#1223,.T.);
#826=FACE_OUTER_BOUND('',#1224,.T.);
#827=FACE_OUTER_BOUND('',#1226,.T.);
#828=FACE_OUTER_BOUND('',#1227,.T.);
#829=FACE_OUTER_BOUND('',#1228,.T.);
#830=FACE_OUTER_BOUND('',#1229,.T.);
#831=FACE_OUTER_BOUND('',#1230,.T.);
#832=FACE_OUTER_BOUND('',#1231,.T.);
#833=FACE_OUTER_BOUND('',#1234,.T.);
#834=FACE_OUTER_BOUND('',#1235,.T.);
#835=FACE_OUTER_BOUND('',#1236,.T.);
#836=FACE_OUTER_BOUND('',#1237,.T.);
#837=FACE_OUTER_BOUND('',#1238,.T.);
#838=FACE_OUTER_BOUND('',#1239,.T.);
#839=FACE_OUTER_BOUND('',#1242,.T.);
#840=FACE_OUTER_BOUND('',#1243,.T.);
#841=FACE_OUTER_BOUND('',#1244,.T.);
#842=FACE_OUTER_BOUND('',#1246,.T.);
#843=FACE_OUTER_BOUND('',#1247,.T.);
#844=FACE_OUTER_BOUND('',#1248,.T.);
#845=FACE_OUTER_BOUND('',#1249,.T.);
#846=FACE_OUTER_BOUND('',#1251,.T.);
#847=FACE_OUTER_BOUND('',#1252,.T.);
#848=FACE_OUTER_BOUND('',#1253,.T.);
#849=FACE_OUTER_BOUND('',#1254,.T.);
#850=FACE_OUTER_BOUND('',#1256,.T.);
#851=FACE_OUTER_BOUND('',#1258,.T.);
#852=FACE_OUTER_BOUND('',#1259,.T.);
#853=FACE_OUTER_BOUND('',#1260,.T.);
#854=FACE_OUTER_BOUND('',#1261,.T.);
#855=FACE_OUTER_BOUND('',#1262,.T.);
#856=FACE_OUTER_BOUND('',#1263,.T.);
#857=FACE_OUTER_BOUND('',#1264,.T.);
#858=FACE_OUTER_BOUND('',#1266,.T.);
#859=FACE_OUTER_BOUND('',#1268,.T.);
#860=FACE_OUTER_BOUND('',#1270,.T.);
#861=FACE_OUTER_BOUND('',#1272,.T.);
#862=FACE_OUTER_BOUND('',#1274,.T.);
#863=FACE_OUTER_BOUND('',#1276,.T.);
#864=FACE_OUTER_BOUND('',#1277,.T.);
#865=FACE_OUTER_BOUND('',#1278,.T.);
#866=FACE_OUTER_BOUND('',#1279,.T.);
#867=FACE_OUTER_BOUND('',#1280,.T.);
#868=FACE_OUTER_BOUND('',#1281,.T.);
#869=FACE_OUTER_BOUND('',#1282,.T.);
#870=FACE_OUTER_BOUND('',#1283,.T.);
#871=FACE_OUTER_BOUND('',#1285,.T.);
#872=FACE_OUTER_BOUND('',#1286,.T.);
#873=FACE_OUTER_BOUND('',#1287,.T.);
#874=FACE_OUTER_BOUND('',#1288,.T.);
#875=FACE_OUTER_BOUND('',#1290,.T.);
#876=FACE_OUTER_BOUND('',#1291,.T.);
#877=FACE_OUTER_BOUND('',#1292,.T.);
#878=FACE_OUTER_BOUND('',#1294,.T.);
#879=FACE_OUTER_BOUND('',#1296,.T.);
#880=FACE_OUTER_BOUND('',#1297,.T.);
#881=FACE_OUTER_BOUND('',#1298,.T.);
#882=FACE_OUTER_BOUND('',#1300,.T.);
#883=FACE_OUTER_BOUND('',#1302,.T.);
#884=FACE_OUTER_BOUND('',#1303,.T.);
#885=FACE_OUTER_BOUND('',#1304,.T.);
#886=FACE_OUTER_BOUND('',#1306,.T.);
#887=FACE_OUTER_BOUND('',#1308,.T.);
#888=FACE_OUTER_BOUND('',#1309,.T.);
#889=FACE_OUTER_BOUND('',#1310,.T.);
#890=FACE_OUTER_BOUND('',#1311,.T.);
#891=FACE_OUTER_BOUND('',#1312,.T.);
#892=FACE_OUTER_BOUND('',#1313,.T.);
#893=FACE_OUTER_BOUND('',#1314,.T.);
#894=FACE_OUTER_BOUND('',#1315,.T.);
#895=FACE_OUTER_BOUND('',#1316,.T.);
#896=FACE_OUTER_BOUND('',#1317,.T.);
#897=FACE_OUTER_BOUND('',#1318,.T.);
#898=FACE_OUTER_BOUND('',#1319,.T.);
#899=FACE_OUTER_BOUND('',#1320,.T.);
#900=FACE_OUTER_BOUND('',#1321,.T.);
#901=FACE_OUTER_BOUND('',#1323,.T.);
#902=FACE_OUTER_BOUND('',#1324,.T.);
#903=FACE_OUTER_BOUND('',#1325,.T.);
#904=FACE_OUTER_BOUND('',#1326,.T.);
#905=FACE_OUTER_BOUND('',#1327,.T.);
#906=FACE_OUTER_BOUND('',#1328,.T.);
#907=FACE_OUTER_BOUND('',#1329,.T.);
#908=FACE_OUTER_BOUND('',#1330,.T.);
#909=FACE_OUTER_BOUND('',#1331,.T.);
#910=FACE_OUTER_BOUND('',#1332,.T.);
#911=FACE_OUTER_BOUND('',#1333,.T.);
#912=FACE_OUTER_BOUND('',#1334,.T.);
#913=FACE_OUTER_BOUND('',#1335,.T.);
#914=FACE_OUTER_BOUND('',#1336,.T.);
#915=FACE_OUTER_BOUND('',#1341,.T.);
#916=FACE_OUTER_BOUND('',#1342,.T.);
#917=FACE_OUTER_BOUND('',#1343,.T.);
#918=FACE_OUTER_BOUND('',#1344,.T.);
#919=FACE_OUTER_BOUND('',#1345,.T.);
#920=FACE_OUTER_BOUND('',#1346,.T.);
#921=FACE_OUTER_BOUND('',#1347,.T.);
#922=FACE_OUTER_BOUND('',#1348,.T.);
#923=FACE_OUTER_BOUND('',#1350,.T.);
#924=FACE_OUTER_BOUND('',#1352,.T.);
#925=FACE_OUTER_BOUND('',#1353,.T.);
#926=FACE_OUTER_BOUND('',#1354,.T.);
#927=FACE_OUTER_BOUND('',#1355,.T.);
#928=FACE_OUTER_BOUND('',#1356,.T.);
#929=FACE_OUTER_BOUND('',#1357,.T.);
#930=FACE_OUTER_BOUND('',#1358,.T.);
#931=FACE_OUTER_BOUND('',#1359,.T.);
#932=FACE_OUTER_BOUND('',#1360,.T.);
#933=FACE_OUTER_BOUND('',#1361,.T.);
#934=FACE_OUTER_BOUND('',#1362,.T.);
#935=FACE_OUTER_BOUND('',#1364,.T.);
#936=FACE_OUTER_BOUND('',#1365,.T.);
#937=FACE_OUTER_BOUND('',#1366,.T.);
#938=FACE_OUTER_BOUND('',#1367,.T.);
#939=FACE_OUTER_BOUND('',#1368,.T.);
#940=FACE_OUTER_BOUND('',#1369,.T.);
#941=FACE_OUTER_BOUND('',#1370,.T.);
#942=FACE_OUTER_BOUND('',#1371,.T.);
#943=FACE_OUTER_BOUND('',#1372,.T.);
#944=FACE_OUTER_BOUND('',#1373,.T.);
#945=FACE_OUTER_BOUND('',#1375,.T.);
#946=FACE_OUTER_BOUND('',#1376,.T.);
#947=FACE_OUTER_BOUND('',#1377,.T.);
#948=FACE_OUTER_BOUND('',#1378,.T.);
#949=FACE_OUTER_BOUND('',#1379,.T.);
#950=FACE_OUTER_BOUND('',#1380,.T.);
#951=FACE_OUTER_BOUND('',#1381,.T.);
#952=FACE_OUTER_BOUND('',#1382,.T.);
#953=FACE_OUTER_BOUND('',#1383,.T.);
#954=FACE_OUTER_BOUND('',#1384,.T.);
#955=FACE_OUTER_BOUND('',#1385,.T.);
#956=FACE_OUTER_BOUND('',#1386,.T.);
#957=FACE_OUTER_BOUND('',#1387,.T.);
#958=FACE_OUTER_BOUND('',#1389,.T.);
#959=FACE_OUTER_BOUND('',#1390,.T.);
#960=FACE_OUTER_BOUND('',#1391,.T.);
#961=FACE_OUTER_BOUND('',#1392,.T.);
#962=FACE_OUTER_BOUND('',#1393,.T.);
#963=FACE_OUTER_BOUND('',#1395,.T.);
#964=FACE_OUTER_BOUND('',#1397,.T.);
#965=FACE_OUTER_BOUND('',#1398,.T.);
#966=FACE_OUTER_BOUND('',#1399,.T.);
#967=FACE_OUTER_BOUND('',#1400,.T.);
#968=FACE_OUTER_BOUND('',#1401,.T.);
#969=FACE_OUTER_BOUND('',#1402,.T.);
#970=FACE_OUTER_BOUND('',#1403,.T.);
#971=FACE_OUTER_BOUND('',#1405,.T.);
#972=FACE_OUTER_BOUND('',#1407,.T.);
#973=FACE_OUTER_BOUND('',#1409,.T.);
#974=FACE_OUTER_BOUND('',#1411,.T.);
#975=FACE_OUTER_BOUND('',#1412,.T.);
#976=FACE_OUTER_BOUND('',#1413,.T.);
#977=FACE_OUTER_BOUND('',#1414,.T.);
#978=FACE_OUTER_BOUND('',#1415,.T.);
#979=FACE_OUTER_BOUND('',#1416,.T.);
#980=FACE_OUTER_BOUND('',#1417,.T.);
#981=FACE_OUTER_BOUND('',#1418,.T.);
#982=FACE_OUTER_BOUND('',#1419,.T.);
#983=FACE_OUTER_BOUND('',#1421,.T.);
#984=FACE_OUTER_BOUND('',#1422,.T.);
#985=EDGE_LOOP('',(#3747,#3748,#3749,#3750));
#986=EDGE_LOOP('',(#3751,#3752,#3753,#3754));
#987=EDGE_LOOP('',(#3755,#3756,#3757,#3758));
#988=EDGE_LOOP('',(#3759,#3760,#3761,#3762));
#989=EDGE_LOOP('',(#3763,#3764,#3765,#3766));
#990=EDGE_LOOP('',(#3767,#3768,#3769,#3770));
#991=EDGE_LOOP('',(#3771,#3772,#3773,#3774));
#992=EDGE_LOOP('',(#3775,#3776,#3777,#3778));
#993=EDGE_LOOP('',(#3779,#3780,#3781,#3782));
#994=EDGE_LOOP('',(#3783));
#995=EDGE_LOOP('',(#3784));
#996=EDGE_LOOP('',(#3785));
#997=EDGE_LOOP('',(#3786));
#998=EDGE_LOOP('',(#3787,#3788,#3789,#3790));
#999=EDGE_LOOP('',(#3791));
#1000=EDGE_LOOP('',(#3792));
#1001=EDGE_LOOP('',(#3793));
#1002=EDGE_LOOP('',(#3794));
#1003=EDGE_LOOP('',(#3795,#3796,#3797,#3798));
#1004=EDGE_LOOP('',(#3799,#3800,#3801,#3802));
#1005=EDGE_LOOP('',(#3803,#3804,#3805,#3806));
#1006=EDGE_LOOP('',(#3807,#3808,#3809,#3810));
#1007=EDGE_LOOP('',(#3811,#3812,#3813,#3814));
#1008=EDGE_LOOP('',(#3815,#3816,#3817,#3818));
#1009=EDGE_LOOP('',(#3819,#3820,#3821,#3822));
#1010=EDGE_LOOP('',(#3823,#3824,#3825,#3826));
#1011=EDGE_LOOP('',(#3827,#3828,#3829,#3830));
#1012=EDGE_LOOP('',(#3831,#3832,#3833,#3834));
#1013=EDGE_LOOP('',(#3835,#3836,#3837,#3838));
#1014=EDGE_LOOP('',(#3839,#3840,#3841,#3842));
#1015=EDGE_LOOP('',(#3843,#3844,#3845,#3846));
#1016=EDGE_LOOP('',(#3847,#3848,#3849,#3850));
#1017=EDGE_LOOP('',(#3851));
#1018=EDGE_LOOP('',(#3852,#3853,#3854,#3855));
#1019=EDGE_LOOP('',(#3856));
#1020=EDGE_LOOP('',(#3857,#3858,#3859,#3860));
#1021=EDGE_LOOP('',(#3861));
#1022=EDGE_LOOP('',(#3862,#3863,#3864,#3865));
#1023=EDGE_LOOP('',(#3866));
#1024=EDGE_LOOP('',(#3867,#3868,#3869,#3870));
#1025=EDGE_LOOP('',(#3871));
#1026=EDGE_LOOP('',(#3872));
#1027=EDGE_LOOP('',(#3873,#3874,#3875,#3876));
#1028=EDGE_LOOP('',(#3877));
#1029=EDGE_LOOP('',(#3878,#3879,#3880,#3881));
#1030=EDGE_LOOP('',(#3882,#3883,#3884,#3885));
#1031=EDGE_LOOP('',(#3886));
#1032=EDGE_LOOP('',(#3887,#3888,#3889,#3890));
#1033=EDGE_LOOP('',(#3891));
#1034=EDGE_LOOP('',(#3892,#3893,#3894,#3895));
#1035=EDGE_LOOP('',(#3896));
#1036=EDGE_LOOP('',(#3897,#3898,#3899,#3900));
#1037=EDGE_LOOP('',(#3901));
#1038=EDGE_LOOP('',(#3902,#3903,#3904,#3905));
#1039=EDGE_LOOP('',(#3906));
#1040=EDGE_LOOP('',(#3907));
#1041=EDGE_LOOP('',(#3908,#3909,#3910,#3911));
#1042=EDGE_LOOP('',(#3912));
#1043=EDGE_LOOP('',(#3913,#3914,#3915,#3916));
#1044=EDGE_LOOP('',(#3917,#3918,#3919,#3920));
#1045=EDGE_LOOP('',(#3921,#3922));
#1046=EDGE_LOOP('',(#3923));
#1047=EDGE_LOOP('',(#3924,#3925,#3926,#3927));
#1048=EDGE_LOOP('',(#3928,#3929,#3930,#3931));
#1049=EDGE_LOOP('',(#3932,#3933));
#1050=EDGE_LOOP('',(#3934));
#1051=EDGE_LOOP('',(#3935,#3936,#3937,#3938));
#1052=EDGE_LOOP('',(#3939,#3940,#3941,#3942));
#1053=EDGE_LOOP('',(#3943,#3944));
#1054=EDGE_LOOP('',(#3945));
#1055=EDGE_LOOP('',(#3946,#3947,#3948,#3949));
#1056=EDGE_LOOP('',(#3950,#3951,#3952,#3953));
#1057=EDGE_LOOP('',(#3954,#3955));
#1058=EDGE_LOOP('',(#3956));
#1059=EDGE_LOOP('',(#3957,#3958,#3959));
#1060=EDGE_LOOP('',(#3960,#3961,#3962));
#1061=EDGE_LOOP('',(#3963,#3964,#3965));
#1062=EDGE_LOOP('',(#3966,#3967,#3968,#3969,#3970,#3971,#3972,#3973));
#1063=EDGE_LOOP('',(#3974));
#1064=EDGE_LOOP('',(#3975));
#1065=EDGE_LOOP('',(#3976));
#1066=EDGE_LOOP('',(#3977));
#1067=EDGE_LOOP('',(#3978));
#1068=EDGE_LOOP('',(#3979));
#1069=EDGE_LOOP('',(#3980));
#1070=EDGE_LOOP('',(#3981));
#1071=EDGE_LOOP('',(#3982));
#1072=EDGE_LOOP('',(#3983));
#1073=EDGE_LOOP('',(#3984,#3985,#3986));
#1074=EDGE_LOOP('',(#3987,#3988,#3989,#3990));
#1075=EDGE_LOOP('',(#3991,#3992,#3993,#3994));
#1076=EDGE_LOOP('',(#3995,#3996,#3997,#3998));
#1077=EDGE_LOOP('',(#3999,#4000,#4001,#4002));
#1078=EDGE_LOOP('',(#4003,#4004,#4005,#4006,#4007,#4008,#4009,#4010,#4011,
#4012));
#1079=EDGE_LOOP('',(#4013,#4014,#4015,#4016,#4017,#4018,#4019,#4020,#4021,
#4022));
#1080=EDGE_LOOP('',(#4023,#4024,#4025,#4026,#4027,#4028,#4029,#4030,#4031,
#4032));
#1081=EDGE_LOOP('',(#4033));
#1082=EDGE_LOOP('',(#4034));
#1083=EDGE_LOOP('',(#4035,#4036,#4037,#4038,#4039,#4040,#4041,#4042,#4043,
#4044));
#1084=EDGE_LOOP('',(#4045,#4046,#4047,#4048));
#1085=EDGE_LOOP('',(#4049));
#1086=EDGE_LOOP('',(#4050));
#1087=EDGE_LOOP('',(#4051));
#1088=EDGE_LOOP('',(#4052));
#1089=EDGE_LOOP('',(#4053));
#1090=EDGE_LOOP('',(#4054));
#1091=EDGE_LOOP('',(#4055,#4056,#4057,#4058));
#1092=EDGE_LOOP('',(#4059,#4060,#4061));
#1093=EDGE_LOOP('',(#4062));
#1094=EDGE_LOOP('',(#4063,#4064));
#1095=EDGE_LOOP('',(#4065));
#1096=EDGE_LOOP('',(#4066,#4067,#4068,#4069));
#1097=EDGE_LOOP('',(#4070,#4071));
#1098=EDGE_LOOP('',(#4072));
#1099=EDGE_LOOP('',(#4073,#4074,#4075,#4076));
#1100=EDGE_LOOP('',(#4077,#4078));
#1101=EDGE_LOOP('',(#4079));
#1102=EDGE_LOOP('',(#4080,#4081,#4082,#4083));
#1103=EDGE_LOOP('',(#4084,#4085,#4086,#4087,#4088,#4089,#4090,#4091));
#1104=EDGE_LOOP('',(#4092));
#1105=EDGE_LOOP('',(#4093,#4094,#4095,#4096));
#1106=EDGE_LOOP('',(#4097,#4098,#4099,#4100));
#1107=EDGE_LOOP('',(#4101,#4102,#4103,#4104));
#1108=EDGE_LOOP('',(#4105,#4106,#4107,#4108));
#1109=EDGE_LOOP('',(#4109,#4110,#4111,#4112));
#1110=EDGE_LOOP('',(#4113));
#1111=EDGE_LOOP('',(#4114));
#1112=EDGE_LOOP('',(#4115,#4116,#4117,#4118));
#1113=EDGE_LOOP('',(#4119,#4120,#4121,#4122,#4123,#4124,#4125,#4126,#4127,
#4128,#4129,#4130,#4131,#4132,#4133,#4134,#4135,#4136,#4137,#4138));
#1114=EDGE_LOOP('',(#4139));
#1115=EDGE_LOOP('',(#4140));
#1116=EDGE_LOOP('',(#4141));
#1117=EDGE_LOOP('',(#4142));
#1118=EDGE_LOOP('',(#4143));
#1119=EDGE_LOOP('',(#4144));
#1120=EDGE_LOOP('',(#4145,#4146,#4147,#4148));
#1121=EDGE_LOOP('',(#4149,#4150,#4151));
#1122=EDGE_LOOP('',(#4152));
#1123=EDGE_LOOP('',(#4153,#4154));
#1124=EDGE_LOOP('',(#4155));
#1125=EDGE_LOOP('',(#4156,#4157,#4158,#4159));
#1126=EDGE_LOOP('',(#4160,#4161));
#1127=EDGE_LOOP('',(#4162));
#1128=EDGE_LOOP('',(#4163,#4164,#4165,#4166));
#1129=EDGE_LOOP('',(#4167,#4168));
#1130=EDGE_LOOP('',(#4169));
#1131=EDGE_LOOP('',(#4170,#4171,#4172,#4173));
#1132=EDGE_LOOP('',(#4174,#4175,#4176,#4177,#4178,#4179,#4180,#4181));
#1133=EDGE_LOOP('',(#4182));
#1134=EDGE_LOOP('',(#4183,#4184,#4185,#4186));
#1135=EDGE_LOOP('',(#4187,#4188,#4189,#4190));
#1136=EDGE_LOOP('',(#4191,#4192,#4193,#4194));
#1137=EDGE_LOOP('',(#4195,#4196,#4197,#4198));
#1138=EDGE_LOOP('',(#4199,#4200,#4201,#4202));
#1139=EDGE_LOOP('',(#4203));
#1140=EDGE_LOOP('',(#4204));
#1141=EDGE_LOOP('',(#4205,#4206,#4207,#4208));
#1142=EDGE_LOOP('',(#4209,#4210,#4211,#4212,#4213,#4214,#4215,#4216,#4217,
#4218,#4219,#4220,#4221,#4222,#4223,#4224,#4225,#4226,#4227,#4228));
#1143=EDGE_LOOP('',(#4229));
#1144=EDGE_LOOP('',(#4230));
#1145=EDGE_LOOP('',(#4231));
#1146=EDGE_LOOP('',(#4232));
#1147=EDGE_LOOP('',(#4233));
#1148=EDGE_LOOP('',(#4234));
#1149=EDGE_LOOP('',(#4235));
#1150=EDGE_LOOP('',(#4236,#4237,#4238,#4239));
#1151=EDGE_LOOP('',(#4240,#4241,#4242,#4243));
#1152=EDGE_LOOP('',(#4244,#4245,#4246,#4247));
#1153=EDGE_LOOP('',(#4248));
#1154=EDGE_LOOP('',(#4249));
#1155=EDGE_LOOP('',(#4250,#4251,#4252,#4253));
#1156=EDGE_LOOP('',(#4254,#4255,#4256,#4257));
#1157=EDGE_LOOP('',(#4258,#4259,#4260,#4261));
#1158=EDGE_LOOP('',(#4262));
#1159=EDGE_LOOP('',(#4263,#4264,#4265,#4266));
#1160=EDGE_LOOP('',(#4267,#4268,#4269,#4270));
#1161=EDGE_LOOP('',(#4271,#4272,#4273,#4274));
#1162=EDGE_LOOP('',(#4275,#4276,#4277,#4278));
#1163=EDGE_LOOP('',(#4279,#4280,#4281,#4282));
#1164=EDGE_LOOP('',(#4283,#4284,#4285,#4286));
#1165=EDGE_LOOP('',(#4287,#4288,#4289,#4290,#4291,#4292));
#1166=EDGE_LOOP('',(#4293,#4294,#4295,#4296,#4297,#4298));
#1167=EDGE_LOOP('',(#4299,#4300,#4301,#4302,#4303,#4304));
#1168=EDGE_LOOP('',(#4305,#4306,#4307,#4308,#4309));
#1169=EDGE_LOOP('',(#4310,#4311,#4312,#4313));
#1170=EDGE_LOOP('',(#4314,#4315,#4316,#4317));
#1171=EDGE_LOOP('',(#4318));
#1172=EDGE_LOOP('',(#4319));
#1173=EDGE_LOOP('',(#4320,#4321,#4322,#4323,#4324));
#1174=EDGE_LOOP('',(#4325));
#1175=EDGE_LOOP('',(#4326));
#1176=EDGE_LOOP('',(#4327,#4328,#4329,#4330));
#1177=EDGE_LOOP('',(#4331,#4332,#4333,#4334,#4335,#4336));
#1178=EDGE_LOOP('',(#4337,#4338,#4339,#4340,#4341));
#1179=EDGE_LOOP('',(#4342));
#1180=EDGE_LOOP('',(#4343));
#1181=EDGE_LOOP('',(#4344,#4345,#4346,#4347));
#1182=EDGE_LOOP('',(#4348,#4349,#4350,#4351));
#1183=EDGE_LOOP('',(#4352,#4353,#4354,#4355));
#1184=EDGE_LOOP('',(#4356));
#1185=EDGE_LOOP('',(#4357));
#1186=EDGE_LOOP('',(#4358,#4359,#4360,#4361,#4362));
#1187=EDGE_LOOP('',(#4363,#4364));
#1188=EDGE_LOOP('',(#4365,#4366));
#1189=EDGE_LOOP('',(#4367,#4368));
#1190=EDGE_LOOP('',(#4369,#4370));
#1191=EDGE_LOOP('',(#4371,#4372));
#1192=EDGE_LOOP('',(#4373,#4374));
#1193=EDGE_LOOP('',(#4375,#4376));
#1194=EDGE_LOOP('',(#4377,#4378));
#1195=EDGE_LOOP('',(#4379,#4380,#4381,#4382));
#1196=EDGE_LOOP('',(#4383,#4384,#4385,#4386,#4387,#4388,#4389,#4390,#4391,
#4392,#4393,#4394,#4395,#4396,#4397,#4398,#4399,#4400,#4401,#4402));
#1197=EDGE_LOOP('',(#4403,#4404,#4405,#4406));
#1198=EDGE_LOOP('',(#4407,#4408,#4409,#4410));
#1199=EDGE_LOOP('',(#4411,#4412,#4413,#4414));
#1200=EDGE_LOOP('',(#4415,#4416,#4417,#4418));
#1201=EDGE_LOOP('',(#4419,#4420,#4421,#4422));
#1202=EDGE_LOOP('',(#4423,#4424,#4425,#4426,#4427,#4428));
#1203=EDGE_LOOP('',(#4429,#4430,#4431,#4432));
#1204=EDGE_LOOP('',(#4433,#4434,#4435,#4436));
#1205=EDGE_LOOP('',(#4437,#4438,#4439,#4440));
#1206=EDGE_LOOP('',(#4441,#4442,#4443,#4444));
#1207=EDGE_LOOP('',(#4445,#4446,#4447,#4448));
#1208=EDGE_LOOP('',(#4449,#4450,#4451,#4452));
#1209=EDGE_LOOP('',(#4453,#4454,#4455,#4456,#4457,#4458,#4459,#4460,#4461,
#4462,#4463,#4464,#4465,#4466,#4467,#4468,#4469,#4470,#4471,#4472));
#1210=EDGE_LOOP('',(#4473,#4474,#4475,#4476));
#1211=EDGE_LOOP('',(#4477,#4478,#4479,#4480));
#1212=EDGE_LOOP('',(#4481));
#1213=EDGE_LOOP('',(#4482));
#1214=EDGE_LOOP('',(#4483,#4484,#4485,#4486));
#1215=EDGE_LOOP('',(#4487));
#1216=EDGE_LOOP('',(#4488));
#1217=EDGE_LOOP('',(#4489,#4490,#4491,#4492));
#1218=EDGE_LOOP('',(#4493));
#1219=EDGE_LOOP('',(#4494));
#1220=EDGE_LOOP('',(#4495,#4496,#4497,#4498));
#1221=EDGE_LOOP('',(#4499));
#1222=EDGE_LOOP('',(#4500));
#1223=EDGE_LOOP('',(#4501,#4502,#4503,#4504));
#1224=EDGE_LOOP('',(#4505));
#1225=EDGE_LOOP('',(#4506));
#1226=EDGE_LOOP('',(#4507,#4508,#4509,#4510));
#1227=EDGE_LOOP('',(#4511,#4512,#4513,#4514));
#1228=EDGE_LOOP('',(#4515));
#1229=EDGE_LOOP('',(#4516,#4517,#4518,#4519));
#1230=EDGE_LOOP('',(#4520,#4521,#4522,#4523));
#1231=EDGE_LOOP('',(#4524,#4525,#4526,#4527,#4528,#4529,#4530,#4531));
#1232=EDGE_LOOP('',(#4532));
#1233=EDGE_LOOP('',(#4533));
#1234=EDGE_LOOP('',(#4534,#4535,#4536,#4537));
#1235=EDGE_LOOP('',(#4538,#4539,#4540,#4541));
#1236=EDGE_LOOP('',(#4542,#4543,#4544,#4545));
#1237=EDGE_LOOP('',(#4546,#4547,#4548,#4549));
#1238=EDGE_LOOP('',(#4550,#4551,#4552,#4553));
#1239=EDGE_LOOP('',(#4554,#4555,#4556,#4557,#4558,#4559,#4560,#4561));
#1240=EDGE_LOOP('',(#4562));
#1241=EDGE_LOOP('',(#4563));
#1242=EDGE_LOOP('',(#4564,#4565,#4566,#4567));
#1243=EDGE_LOOP('',(#4568,#4569,#4570,#4571));
#1244=EDGE_LOOP('',(#4572));
#1245=EDGE_LOOP('',(#4573));
#1246=EDGE_LOOP('',(#4574,#4575,#4576,#4577));
#1247=EDGE_LOOP('',(#4578,#4579,#4580,#4581));
#1248=EDGE_LOOP('',(#4582,#4583,#4584,#4585));
#1249=EDGE_LOOP('',(#4586));
#1250=EDGE_LOOP('',(#4587));
#1251=EDGE_LOOP('',(#4588));
#1252=EDGE_LOOP('',(#4589,#4590,#4591,#4592));
#1253=EDGE_LOOP('',(#4593,#4594,#4595,#4596));
#1254=EDGE_LOOP('',(#4597));
#1255=EDGE_LOOP('',(#4598));
#1256=EDGE_LOOP('',(#4599));
#1257=EDGE_LOOP('',(#4600));
#1258=EDGE_LOOP('',(#4601,#4602,#4603));
#1259=EDGE_LOOP('',(#4604,#4605,#4606,#4607,#4608,#4609,#4610,#4611));
#1260=EDGE_LOOP('',(#4612,#4613));
#1261=EDGE_LOOP('',(#4614,#4615));
#1262=EDGE_LOOP('',(#4616,#4617,#4618,#4619,#4620,#4621,#4622,#4623,#4624,
#4625,#4626));
#1263=EDGE_LOOP('',(#4627,#4628));
#1264=EDGE_LOOP('',(#4629,#4630,#4631,#4632,#4633,#4634,#4635,#4636,#4637,
#4638,#4639,#4640));
#1265=EDGE_LOOP('',(#4641,#4642,#4643,#4644));
#1266=EDGE_LOOP('',(#4645,#4646,#4647,#4648,#4649,#4650,#4651,#4652,#4653));
#1267=EDGE_LOOP('',(#4654));
#1268=EDGE_LOOP('',(#4655));
#1269=EDGE_LOOP('',(#4656));
#1270=EDGE_LOOP('',(#4657));
#1271=EDGE_LOOP('',(#4658));
#1272=EDGE_LOOP('',(#4659));
#1273=EDGE_LOOP('',(#4660));
#1274=EDGE_LOOP('',(#4661));
#1275=EDGE_LOOP('',(#4662));
#1276=EDGE_LOOP('',(#4663,#4664,#4665,#4666));
#1277=EDGE_LOOP('',(#4667,#4668,#4669,#4670));
#1278=EDGE_LOOP('',(#4671,#4672,#4673,#4674));
#1279=EDGE_LOOP('',(#4675));
#1280=EDGE_LOOP('',(#4676));
#1281=EDGE_LOOP('',(#4677,#4678,#4679,#4680));
#1282=EDGE_LOOP('',(#4681,#4682,#4683,#4684));
#1283=EDGE_LOOP('',(#4685,#4686,#4687,#4688));
#1284=EDGE_LOOP('',(#4689));
#1285=EDGE_LOOP('',(#4690,#4691,#4692,#4693));
#1286=EDGE_LOOP('',(#4694,#4695,#4696,#4697));
#1287=EDGE_LOOP('',(#4698,#4699,#4700,#4701));
#1288=EDGE_LOOP('',(#4702,#4703,#4704,#4705));
#1289=EDGE_LOOP('',(#4706));
#1290=EDGE_LOOP('',(#4707,#4708,#4709,#4710));
#1291=EDGE_LOOP('',(#4711,#4712,#4713,#4714));
#1292=EDGE_LOOP('',(#4715));
#1293=EDGE_LOOP('',(#4716));
#1294=EDGE_LOOP('',(#4717));
#1295=EDGE_LOOP('',(#4718));
#1296=EDGE_LOOP('',(#4719,#4720,#4721,#4722));
#1297=EDGE_LOOP('',(#4723,#4724,#4725,#4726));
#1298=EDGE_LOOP('',(#4727));
#1299=EDGE_LOOP('',(#4728));
#1300=EDGE_LOOP('',(#4729));
#1301=EDGE_LOOP('',(#4730));
#1302=EDGE_LOOP('',(#4731,#4732,#4733,#4734));
#1303=EDGE_LOOP('',(#4735,#4736,#4737,#4738));
#1304=EDGE_LOOP('',(#4739));
#1305=EDGE_LOOP('',(#4740));
#1306=EDGE_LOOP('',(#4741));
#1307=EDGE_LOOP('',(#4742));
#1308=EDGE_LOOP('',(#4743,#4744,#4745,#4746));
#1309=EDGE_LOOP('',(#4747,#4748,#4749,#4750));
#1310=EDGE_LOOP('',(#4751,#4752,#4753,#4754));
#1311=EDGE_LOOP('',(#4755,#4756,#4757,#4758));
#1312=EDGE_LOOP('',(#4759,#4760,#4761,#4762));
#1313=EDGE_LOOP('',(#4763,#4764,#4765,#4766));
#1314=EDGE_LOOP('',(#4767,#4768,#4769,#4770,#4771,#4772));
#1315=EDGE_LOOP('',(#4773,#4774,#4775,#4776,#4777,#4778));
#1316=EDGE_LOOP('',(#4779));
#1317=EDGE_LOOP('',(#4780));
#1318=EDGE_LOOP('',(#4781,#4782,#4783,#4784));
#1319=EDGE_LOOP('',(#4785,#4786,#4787,#4788));
#1320=EDGE_LOOP('',(#4789,#4790,#4791,#4792));
#1321=EDGE_LOOP('',(#4793));
#1322=EDGE_LOOP('',(#4794));
#1323=EDGE_LOOP('',(#4795,#4796,#4797,#4798));
#1324=EDGE_LOOP('',(#4799,#4800,#4801,#4802));
#1325=EDGE_LOOP('',(#4803,#4804,#4805,#4806));
#1326=EDGE_LOOP('',(#4807,#4808,#4809,#4810));
#1327=EDGE_LOOP('',(#4811,#4812,#4813,#4814));
#1328=EDGE_LOOP('',(#4815,#4816,#4817,#4818));
#1329=EDGE_LOOP('',(#4819,#4820,#4821,#4822));
#1330=EDGE_LOOP('',(#4823,#4824,#4825,#4826));
#1331=EDGE_LOOP('',(#4827,#4828,#4829,#4830));
#1332=EDGE_LOOP('',(#4831,#4832,#4833,#4834));
#1333=EDGE_LOOP('',(#4835,#4836,#4837,#4838));
#1334=EDGE_LOOP('',(#4839,#4840,#4841,#4842));
#1335=EDGE_LOOP('',(#4843,#4844,#4845,#4846));
#1336=EDGE_LOOP('',(#4847,#4848,#4849,#4850,#4851,#4852,#4853,#4854,#4855,
#4856,#4857,#4858,#4859,#4860,#4861,#4862,#4863,#4864,#4865,#4866,#4867,
#4868,#4869,#4870,#4871,#4872,#4873,#4874,#4875,#4876,#4877,#4878,#4879,
#4880,#4881,#4882,#4883,#4884,#4885,#4886));
#1337=EDGE_LOOP('',(#4887));
#1338=EDGE_LOOP('',(#4888));
#1339=EDGE_LOOP('',(#4889));
#1340=EDGE_LOOP('',(#4890));
#1341=EDGE_LOOP('',(#4891,#4892,#4893,#4894));
#1342=EDGE_LOOP('',(#4895,#4896,#4897,#4898));
#1343=EDGE_LOOP('',(#4899,#4900,#4901,#4902));
#1344=EDGE_LOOP('',(#4903,#4904,#4905,#4906));
#1345=EDGE_LOOP('',(#4907,#4908,#4909,#4910));
#1346=EDGE_LOOP('',(#4911,#4912,#4913,#4914));
#1347=EDGE_LOOP('',(#4915,#4916,#4917,#4918));
#1348=EDGE_LOOP('',(#4919,#4920,#4921,#4922,#4923,#4924,#4925,#4926,#4927,
#4928,#4929,#4930));
#1349=EDGE_LOOP('',(#4931));
#1350=EDGE_LOOP('',(#4932,#4933,#4934,#4935,#4936,#4937,#4938,#4939,#4940,
#4941,#4942,#4943));
#1351=EDGE_LOOP('',(#4944));
#1352=EDGE_LOOP('',(#4945,#4946));
#1353=EDGE_LOOP('',(#4947,#4948,#4949,#4950,#4951,#4952,#4953,#4954));
#1354=EDGE_LOOP('',(#4955,#4956,#4957,#4958,#4959,#4960,#4961,#4962,#4963,
#4964,#4965,#4966,#4967,#4968,#4969,#4970,#4971,#4972,#4973,#4974));
#1355=EDGE_LOOP('',(#4975,#4976,#4977,#4978));
#1356=EDGE_LOOP('',(#4979,#4980,#4981,#4982));
#1357=EDGE_LOOP('',(#4983,#4984,#4985,#4986));
#1358=EDGE_LOOP('',(#4987,#4988,#4989,#4990));
#1359=EDGE_LOOP('',(#4991,#4992,#4993,#4994));
#1360=EDGE_LOOP('',(#4995,#4996,#4997,#4998));
#1361=EDGE_LOOP('',(#4999,#5000,#5001,#5002));
#1362=EDGE_LOOP('',(#5003,#5004,#5005,#5006,#5007,#5008,#5009,#5010,#5011,
#5012,#5013,#5014));
#1363=EDGE_LOOP('',(#5015));
#1364=EDGE_LOOP('',(#5016,#5017,#5018));
#1365=EDGE_LOOP('',(#5019,#5020,#5021,#5022,#5023,#5024,#5025,#5026));
#1366=EDGE_LOOP('',(#5027,#5028,#5029,#5030));
#1367=EDGE_LOOP('',(#5031,#5032,#5033,#5034));
#1368=EDGE_LOOP('',(#5035,#5036,#5037,#5038));
#1369=EDGE_LOOP('',(#5039,#5040,#5041,#5042));
#1370=EDGE_LOOP('',(#5043,#5044,#5045,#5046));
#1371=EDGE_LOOP('',(#5047,#5048,#5049,#5050));
#1372=EDGE_LOOP('',(#5051,#5052,#5053,#5054));
#1373=EDGE_LOOP('',(#5055,#5056,#5057,#5058,#5059,#5060,#5061,#5062,#5063,
#5064,#5065,#5066));
#1374=EDGE_LOOP('',(#5067));
#1375=EDGE_LOOP('',(#5068,#5069));
#1376=EDGE_LOOP('',(#5070,#5071,#5072,#5073,#5074,#5075,#5076,#5077));
#1377=EDGE_LOOP('',(#5078,#5079,#5080,#5081));
#1378=EDGE_LOOP('',(#5082,#5083,#5084,#5085));
#1379=EDGE_LOOP('',(#5086,#5087,#5088,#5089));
#1380=EDGE_LOOP('',(#5090,#5091,#5092,#5093));
#1381=EDGE_LOOP('',(#5094,#5095,#5096,#5097));
#1382=EDGE_LOOP('',(#5098,#5099,#5100,#5101));
#1383=EDGE_LOOP('',(#5102,#5103));
#1384=EDGE_LOOP('',(#5104,#5105,#5106,#5107,#5108,#5109,#5110,#5111));
#1385=EDGE_LOOP('',(#5112,#5113,#5114,#5115));
#1386=EDGE_LOOP('',(#5116,#5117,#5118,#5119));
#1387=EDGE_LOOP('',(#5120));
#1388=EDGE_LOOP('',(#5121));
#1389=EDGE_LOOP('',(#5122,#5123,#5124,#5125));
#1390=EDGE_LOOP('',(#5126));
#1391=EDGE_LOOP('',(#5127,#5128,#5129,#5130));
#1392=EDGE_LOOP('',(#5131,#5132,#5133,#5134));
#1393=EDGE_LOOP('',(#5135));
#1394=EDGE_LOOP('',(#5136));
#1395=EDGE_LOOP('',(#5137));
#1396=EDGE_LOOP('',(#5138));
#1397=EDGE_LOOP('',(#5139,#5140,#5141));
#1398=EDGE_LOOP('',(#5142,#5143,#5144,#5145,#5146,#5147,#5148,#5149));
#1399=EDGE_LOOP('',(#5150,#5151));
#1400=EDGE_LOOP('',(#5152,#5153));
#1401=EDGE_LOOP('',(#5154,#5155,#5156,#5157,#5158,#5159,#5160,#5161,#5162,
#5163,#5164));
#1402=EDGE_LOOP('',(#5165,#5166));
#1403=EDGE_LOOP('',(#5167,#5168,#5169,#5170,#5171,#5172,#5173,#5174,#5175,
#5176,#5177,#5178));
#1404=EDGE_LOOP('',(#5179,#5180,#5181,#5182));
#1405=EDGE_LOOP('',(#5183,#5184,#5185,#5186,#5187,#5188,#5189,#5190,#5191));
#1406=EDGE_LOOP('',(#5192));
#1407=EDGE_LOOP('',(#5193));
#1408=EDGE_LOOP('',(#5194));
#1409=EDGE_LOOP('',(#5195));
#1410=EDGE_LOOP('',(#5196));
#1411=EDGE_LOOP('',(#5197));
#1412=EDGE_LOOP('',(#5198,#5199,#5200,#5201));
#1413=EDGE_LOOP('',(#5202,#5203,#5204,#5205));
#1414=EDGE_LOOP('',(#5206,#5207,#5208,#5209));
#1415=EDGE_LOOP('',(#5210,#5211,#5212,#5213));
#1416=EDGE_LOOP('',(#5214,#5215,#5216,#5217));
#1417=EDGE_LOOP('',(#5218,#5219,#5220,#5221));
#1418=EDGE_LOOP('',(#5222,#5223,#5224,#5225,#5226,#5227));
#1419=EDGE_LOOP('',(#5228));
#1420=EDGE_LOOP('',(#5229,#5230,#5231,#5232,#5233,#5234));
#1421=EDGE_LOOP('',(#5235,#5236,#5237,#5238));
#1422=EDGE_LOOP('',(#5239,#5240,#5241,#5242));
#1423=LINE('',#8608,#1797);
#1424=LINE('',#8614,#1798);
#1425=LINE('',#8620,#1799);
#1426=LINE('',#8626,#1800);
#1427=LINE('',#8631,#1801);
#1428=LINE('',#8633,#1802);
#1429=LINE('',#8635,#1803);
#1430=LINE('',#8636,#1804);
#1431=LINE('',#8639,#1805);
#1432=LINE('',#8641,#1806);
#1433=LINE('',#8642,#1807);
#1434=LINE('',#8645,#1808);
#1435=LINE('',#8647,#1809);
#1436=LINE('',#8648,#1810);
#1437=LINE('',#8650,#1811);
#1438=LINE('',#8651,#1812);
#1439=LINE('',#8658,#1813);
#1440=LINE('',#8660,#1814);
#1441=LINE('',#8662,#1815);
#1442=LINE('',#8663,#1816);
#1443=LINE('',#8666,#1817);
#1444=LINE('',#8668,#1818);
#1445=LINE('',#8669,#1819);
#1446=LINE('',#8672,#1820);
#1447=LINE('',#8674,#1821);
#1448=LINE('',#8675,#1822);
#1449=LINE('',#8677,#1823);
#1450=LINE('',#8678,#1824);
#1451=LINE('',#8685,#1825);
#1452=LINE('',#8687,#1826);
#1453=LINE('',#8689,#1827);
#1454=LINE('',#8690,#1828);
#1455=LINE('',#8693,#1829);
#1456=LINE('',#8695,#1830);
#1457=LINE('',#8696,#1831);
#1458=LINE('',#8699,#1832);
#1459=LINE('',#8701,#1833);
#1460=LINE('',#8702,#1834);
#1461=LINE('',#8704,#1835);
#1462=LINE('',#8705,#1836);
#1463=LINE('',#8713,#1837);
#1464=LINE('',#8752,#1838);
#1465=LINE('',#8759,#1839);
#1466=LINE('',#8766,#1840);
#1467=LINE('',#8773,#1841);
#1468=LINE('',#8780,#1842);
#1469=LINE('',#8788,#1843);
#1470=LINE('',#8793,#1844);
#1471=LINE('',#8832,#1845);
#1472=LINE('',#8839,#1846);
#1473=LINE('',#8846,#1847);
#1474=LINE('',#8853,#1848);
#1475=LINE('',#8860,#1849);
#1476=LINE('',#8868,#1850);
#1477=LINE('',#8872,#1851);
#1478=LINE('',#8876,#1852);
#1479=LINE('',#8879,#1853);
#1480=LINE('',#8881,#1854);
#1481=LINE('',#8889,#1855);
#1482=LINE('',#8893,#1856);
#1483=LINE('',#8896,#1857);
#1484=LINE('',#8898,#1858);
#1485=LINE('',#8906,#1859);
#1486=LINE('',#8910,#1860);
#1487=LINE('',#8913,#1861);
#1488=LINE('',#8915,#1862);
#1489=LINE('',#8923,#1863);
#1490=LINE('',#8927,#1864);
#1491=LINE('',#8930,#1865);
#1492=LINE('',#8932,#1866);
#1493=LINE('',#8939,#1867);
#1494=LINE('',#8940,#1868);
#1495=LINE('',#8943,#1869);
#1496=LINE('',#8944,#1870);
#1497=LINE('',#8947,#1871);
#1498=LINE('',#8948,#1872);
#1499=LINE('',#8950,#1873);
#1500=LINE('',#8951,#1874);
#1501=LINE('',#8952,#1875);
#1502=LINE('',#8953,#1876);
#1503=LINE('',#8956,#1877);
#1504=LINE('',#8957,#1878);
#1505=LINE('',#8961,#1879);
#1506=LINE('',#8965,#1880);
#1507=LINE('',#8969,#1881);
#1508=LINE('',#8973,#1882);
#1509=LINE('',#8977,#1883);
#1510=LINE('',#8978,#1884);
#1511=LINE('',#8979,#1885);
#1512=LINE('',#8982,#1886);
#1513=LINE('',#8983,#1887);
#1514=LINE('',#8986,#1888);
#1515=LINE('',#8987,#1889);
#1516=LINE('',#8989,#1890);
#1517=LINE('',#8995,#1891);
#1518=LINE('',#8999,#1892);
#1519=LINE('',#9016,#1893);
#1520=LINE('',#9019,#1894);
#1521=LINE('',#9029,#1895);
#1522=LINE('',#9032,#1896);
#1523=LINE('',#9042,#1897);
#1524=LINE('',#9045,#1898);
#1525=LINE('',#9056,#1899);
#1526=LINE('',#9060,#1900);
#1527=LINE('',#9064,#1901);
#1528=LINE('',#9068,#1902);
#1529=LINE('',#9073,#1903);
#1530=LINE('',#9079,#1904);
#1531=LINE('',#9082,#1905);
#1532=LINE('',#9089,#1906);
#1533=LINE('',#9093,#1907);
#1534=LINE('',#9110,#1908);
#1535=LINE('',#9113,#1909);
#1536=LINE('',#9123,#1910);
#1537=LINE('',#9126,#1911);
#1538=LINE('',#9136,#1912);
#1539=LINE('',#9139,#1913);
#1540=LINE('',#9150,#1914);
#1541=LINE('',#9154,#1915);
#1542=LINE('',#9158,#1916);
#1543=LINE('',#9162,#1917);
#1544=LINE('',#9167,#1918);
#1545=LINE('',#9173,#1919);
#1546=LINE('',#9176,#1920);
#1547=LINE('',#9186,#1921);
#1548=LINE('',#9190,#1922);
#1549=LINE('',#9194,#1923);
#1550=LINE('',#9201,#1924);
#1551=LINE('',#9205,#1925);
#1552=LINE('',#9209,#1926);
#1553=LINE('',#9214,#1927);
#1554=LINE('',#9216,#1928);
#1555=LINE('',#9218,#1929);
#1556=LINE('',#9219,#1930);
#1557=LINE('',#9222,#1931);
#1558=LINE('',#9224,#1932);
#1559=LINE('',#9225,#1933);
#1560=LINE('',#9228,#1934);
#1561=LINE('',#9230,#1935);
#1562=LINE('',#9231,#1936);
#1563=LINE('',#9234,#1937);
#1564=LINE('',#9236,#1938);
#1565=LINE('',#9237,#1939);
#1566=LINE('',#9240,#1940);
#1567=LINE('',#9242,#1941);
#1568=LINE('',#9243,#1942);
#1569=LINE('',#9245,#1943);
#1570=LINE('',#9246,#1944);
#1571=LINE('',#9263,#1945);
#1572=LINE('',#9269,#1946);
#1573=LINE('',#9273,#1947);
#1574=LINE('',#9279,#1948);
#1575=LINE('',#9284,#1949);
#1576=LINE('',#9299,#1950);
#1577=LINE('',#9308,#1951);
#1578=LINE('',#9312,#1952);
#1579=LINE('',#9316,#1953);
#1580=LINE('',#9319,#1954);
#1581=LINE('',#9472,#1955);
#1582=LINE('',#9768,#1956);
#1583=LINE('',#9810,#1957);
#1584=LINE('',#9815,#1958);
#1585=LINE('',#9824,#1959);
#1586=LINE('',#9829,#1960);
#1587=LINE('',#9841,#1961);
#1588=LINE('',#9848,#1962);
#1589=LINE('',#9853,#1963);
#1590=LINE('',#9857,#1964);
#1591=LINE('',#9861,#1965);
#1592=LINE('',#9865,#1966);
#1593=LINE('',#9867,#1967);
#1594=LINE('',#9869,#1968);
#1595=LINE('',#9872,#1969);
#1596=LINE('',#9877,#1970);
#1597=LINE('',#9878,#1971);
#1598=LINE('',#9881,#1972);
#1599=LINE('',#9882,#1973);
#1600=LINE('',#9885,#1974);
#1601=LINE('',#9887,#1975);
#1602=LINE('',#9888,#1976);
#1603=LINE('',#9891,#1977);
#1604=LINE('',#9893,#1978);
#1605=LINE('',#9894,#1979);
#1606=LINE('',#9896,#1980);
#1607=LINE('',#9910,#1981);
#1608=LINE('',#9913,#1982);
#1609=LINE('',#9918,#1983);
#1610=LINE('',#9926,#1984);
#1611=LINE('',#9932,#1985);
#1612=LINE('',#9940,#1986);
#1613=LINE('',#9980,#1987);
#1614=LINE('',#10013,#1988);
#1615=LINE('',#10017,#1989);
#1616=LINE('',#10062,#1990);
#1617=LINE('',#10100,#1991);
#1618=LINE('',#10104,#1992);
#1619=LINE('',#10106,#1993);
#1620=LINE('',#10111,#1994);
#1621=LINE('',#10113,#1995);
#1622=LINE('',#10129,#1996);
#1623=LINE('',#10132,#1997);
#1624=LINE('',#10137,#1998);
#1625=LINE('',#10145,#1999);
#1626=LINE('',#10150,#2000);
#1627=LINE('',#10154,#2001);
#1628=LINE('',#10158,#2002);
#1629=LINE('',#10161,#2003);
#1630=LINE('',#10164,#2004);
#1631=LINE('',#10165,#2005);
#1632=LINE('',#10168,#2006);
#1633=LINE('',#10169,#2007);
#1634=LINE('',#10178,#2008);
#1635=LINE('',#10184,#2009);
#1636=LINE('',#10193,#2010);
#1637=LINE('',#10199,#2011);
#1638=LINE('',#10208,#2012);
#1639=LINE('',#10214,#2013);
#1640=LINE('',#10222,#2014);
#1641=LINE('',#10224,#2015);
#1642=LINE('',#10226,#2016);
#1643=LINE('',#10227,#2017);
#1644=LINE('',#10230,#2018);
#1645=LINE('',#10232,#2019);
#1646=LINE('',#10233,#2020);
#1647=LINE('',#10236,#2021);
#1648=LINE('',#10238,#2022);
#1649=LINE('',#10239,#2023);
#1650=LINE('',#10242,#2024);
#1651=LINE('',#10244,#2025);
#1652=LINE('',#10245,#2026);
#1653=LINE('',#10248,#2027);
#1654=LINE('',#10250,#2028);
#1655=LINE('',#10251,#2029);
#1656=LINE('',#10253,#2030);
#1657=LINE('',#10254,#2031);
#1658=LINE('',#10266,#2032);
#1659=LINE('',#10270,#2033);
#1660=LINE('',#10274,#2034);
#1661=LINE('',#10281,#2035);
#1662=LINE('',#10283,#2036);
#1663=LINE('',#10310,#2037);
#1664=LINE('',#10316,#2038);
#1665=LINE('',#10322,#2039);
#1666=LINE('',#10328,#2040);
#1667=LINE('',#10335,#2041);
#1668=LINE('',#10338,#2042);
#1669=LINE('',#10344,#2043);
#1670=LINE('',#10347,#2044);
#1671=LINE('',#10353,#2045);
#1672=LINE('',#10356,#2046);
#1673=LINE('',#10360,#2047);
#1674=LINE('',#10364,#2048);
#1675=LINE('',#10370,#2049);
#1676=LINE('',#10376,#2050);
#1677=LINE('',#10382,#2051);
#1678=LINE('',#10386,#2052);
#1679=LINE('',#10388,#2053);
#1680=LINE('',#10390,#2054);
#1681=LINE('',#10394,#2055);
#1682=LINE('',#10396,#2056);
#1683=LINE('',#10398,#2057);
#1684=LINE('',#10403,#2058);
#1685=LINE('',#10405,#2059);
#1686=LINE('',#10407,#2060);
#1687=LINE('',#10411,#2061);
#1688=LINE('',#10413,#2062);
#1689=LINE('',#10415,#2063);
#1690=LINE('',#10418,#2064);
#1691=LINE('',#10420,#2065);
#1692=LINE('',#10422,#2066);
#1693=LINE('',#10426,#2067);
#1694=LINE('',#10428,#2068);
#1695=LINE('',#10430,#2069);
#1696=LINE('',#10433,#2070);
#1697=LINE('',#10435,#2071);
#1698=LINE('',#10437,#2072);
#1699=LINE('',#10441,#2073);
#1700=LINE('',#10443,#2074);
#1701=LINE('',#10445,#2075);
#1702=LINE('',#10450,#2076);
#1703=LINE('',#10453,#2077);
#1704=LINE('',#10457,#2078);
#1705=LINE('',#10458,#2079);
#1706=LINE('',#10461,#2080);
#1707=LINE('',#10462,#2081);
#1708=LINE('',#10465,#2082);
#1709=LINE('',#10467,#2083);
#1710=LINE('',#10468,#2084);
#1711=LINE('',#10470,#2085);
#1712=LINE('',#10473,#2086);
#1713=LINE('',#10474,#2087);
#1714=LINE('',#10479,#2088);
#1715=LINE('',#10481,#2089);
#1716=LINE('',#10483,#2090);
#1717=LINE('',#10491,#2091);
#1718=LINE('',#10499,#2092);
#1719=LINE('',#10501,#2093);
#1720=LINE('',#10502,#2094);
#1721=LINE('',#10509,#2095);
#1722=LINE('',#10510,#2096);
#1723=LINE('',#10511,#2097);
#1724=LINE('',#10514,#2098);
#1725=LINE('',#10518,#2099);
#1726=LINE('',#10523,#2100);
#1727=LINE('',#10527,#2101);
#1728=LINE('',#10531,#2102);
#1729=LINE('',#10535,#2103);
#1730=LINE('',#10538,#2104);
#1731=LINE('',#10541,#2105);
#1732=LINE('',#10543,#2106);
#1733=LINE('',#10545,#2107);
#1734=LINE('',#10548,#2108);
#1735=LINE('',#10550,#2109);
#1736=LINE('',#10551,#2110);
#1737=LINE('',#10553,#2111);
#1738=LINE('',#10556,#2112);
#1739=LINE('',#10557,#2113);
#1740=LINE('',#10562,#2114);
#1741=LINE('',#10564,#2115);
#1742=LINE('',#10566,#2116);
#1743=LINE('',#10572,#2117);
#1744=LINE('',#10575,#2118);
#1745=LINE('',#10577,#2119);
#1746=LINE('',#10579,#2120);
#1747=LINE('',#10582,#2121);
#1748=LINE('',#10584,#2122);
#1749=LINE('',#10585,#2123);
#1750=LINE('',#10587,#2124);
#1751=LINE('',#10590,#2125);
#1752=LINE('',#10591,#2126);
#1753=LINE('',#10596,#2127);
#1754=LINE('',#10598,#2128);
#1755=LINE('',#10600,#2129);
#1756=LINE('',#10606,#2130);
#1757=LINE('',#10609,#2131);
#1758=LINE('',#10611,#2132);
#1759=LINE('',#10613,#2133);
#1760=LINE('',#10615,#2134);
#1761=LINE('',#10617,#2135);
#1762=LINE('',#10621,#2136);
#1763=LINE('',#10622,#2137);
#1764=LINE('',#10630,#2138);
#1765=LINE('',#10638,#2139);
#1766=LINE('',#10644,#2140);
#1767=LINE('',#10652,#2141);
#1768=LINE('',#10692,#2142);
#1769=LINE('',#10725,#2143);
#1770=LINE('',#10729,#2144);
#1771=LINE('',#10774,#2145);
#1772=LINE('',#10812,#2146);
#1773=LINE('',#10816,#2147);
#1774=LINE('',#10818,#2148);
#1775=LINE('',#10823,#2149);
#1776=LINE('',#10825,#2150);
#1777=LINE('',#10836,#2151);
#1778=LINE('',#10838,#2152);
#1779=LINE('',#10840,#2153);
#1780=LINE('',#10841,#2154);
#1781=LINE('',#10844,#2155);
#1782=LINE('',#10846,#2156);
#1783=LINE('',#10847,#2157);
#1784=LINE('',#10850,#2158);
#1785=LINE('',#10852,#2159);
#1786=LINE('',#10853,#2160);
#1787=LINE('',#10856,#2161);
#1788=LINE('',#10858,#2162);
#1789=LINE('',#10859,#2163);
#1790=LINE('',#10862,#2164);
#1791=LINE('',#10864,#2165);
#1792=LINE('',#10865,#2166);
#1793=LINE('',#10867,#2167);
#1794=LINE('',#10868,#2168);
#1795=LINE('',#10876,#2169);
#1796=LINE('',#10878,#2170);
#1797=VECTOR('',#6759,0.21);
#1798=VECTOR('',#6766,0.21);
#1799=VECTOR('',#6773,0.21);
#1800=VECTOR('',#6780,0.21);
#1801=VECTOR('',#6785,1.);
#1802=VECTOR('',#6786,1.);
#1803=VECTOR('',#6787,1.);
#1804=VECTOR('',#6788,1.);
#1805=VECTOR('',#6791,1.);
#1806=VECTOR('',#6792,1.);
#1807=VECTOR('',#6793,1.);
#1808=VECTOR('',#6796,1.);
#1809=VECTOR('',#6797,1.);
#1810=VECTOR('',#6798,1.);
#1811=VECTOR('',#6801,1.);
#1812=VECTOR('',#6802,1.);
#1813=VECTOR('',#6811,1.);
#1814=VECTOR('',#6812,1.);
#1815=VECTOR('',#6813,1.);
#1816=VECTOR('',#6814,1.);
#1817=VECTOR('',#6817,1.);
#1818=VECTOR('',#6818,1.);
#1819=VECTOR('',#6819,1.);
#1820=VECTOR('',#6822,1.);
#1821=VECTOR('',#6823,1.);
#1822=VECTOR('',#6824,1.);
#1823=VECTOR('',#6827,1.);
#1824=VECTOR('',#6828,1.);
#1825=VECTOR('',#6837,1.);
#1826=VECTOR('',#6838,1.);
#1827=VECTOR('',#6839,1.);
#1828=VECTOR('',#6840,1.);
#1829=VECTOR('',#6843,1.);
#1830=VECTOR('',#6844,1.);
#1831=VECTOR('',#6845,1.);
#1832=VECTOR('',#6848,1.);
#1833=VECTOR('',#6849,1.);
#1834=VECTOR('',#6850,1.);
#1835=VECTOR('',#6853,1.);
#1836=VECTOR('',#6854,1.);
#1837=VECTOR('',#6865,0.25);
#1838=VECTOR('',#6870,0.165);
#1839=VECTOR('',#6879,0.165);
#1840=VECTOR('',#6888,0.165);
#1841=VECTOR('',#6897,0.165);
#1842=VECTOR('',#6906,1.5);
#1843=VECTOR('',#6917,1.02);
#1844=VECTOR('',#6922,0.25);
#1845=VECTOR('',#6927,0.165);
#1846=VECTOR('',#6936,0.165);
#1847=VECTOR('',#6945,0.165);
#1848=VECTOR('',#6954,0.165);
#1849=VECTOR('',#6963,1.5);
#1850=VECTOR('',#6974,1.02);
#1851=VECTOR('',#6977,1.);
#1852=VECTOR('',#6980,1.);
#1853=VECTOR('',#6985,1.);
#1854=VECTOR('',#6988,1.);
#1855=VECTOR('',#6997,1.);
#1856=VECTOR('',#7000,1.);
#1857=VECTOR('',#7005,1.);
#1858=VECTOR('',#7008,1.);
#1859=VECTOR('',#7017,1.);
#1860=VECTOR('',#7020,1.);
#1861=VECTOR('',#7025,1.);
#1862=VECTOR('',#7028,1.);
#1863=VECTOR('',#7037,1.);
#1864=VECTOR('',#7040,1.);
#1865=VECTOR('',#7045,1.);
#1866=VECTOR('',#7048,1.);
#1867=VECTOR('',#7057,1.);
#1868=VECTOR('',#7058,1.);
#1869=VECTOR('',#7061,1.);
#1870=VECTOR('',#7062,1.);
#1871=VECTOR('',#7065,1.);
#1872=VECTOR('',#7066,1.);
#1873=VECTOR('',#7069,1.);
#1874=VECTOR('',#7070,1.);
#1875=VECTOR('',#7071,1.);
#1876=VECTOR('',#7072,1.);
#1877=VECTOR('',#7075,1.);
#1878=VECTOR('',#7076,1.);
#1879=VECTOR('',#7081,0.275);
#1880=VECTOR('',#7086,0.275);
#1881=VECTOR('',#7091,0.275);
#1882=VECTOR('',#7096,0.275);
#1883=VECTOR('',#7099,1.);
#1884=VECTOR('',#7100,1.);
#1885=VECTOR('',#7101,1.);
#1886=VECTOR('',#7104,1.);
#1887=VECTOR('',#7105,1.);
#1888=VECTOR('',#7108,1.);
#1889=VECTOR('',#7109,1.);
#1890=VECTOR('',#7112,1.);
#1891=VECTOR('',#7119,1.);
#1892=VECTOR('',#7122,1.);
#1893=VECTOR('',#7143,1.);
#1894=VECTOR('',#7146,1.);
#1895=VECTOR('',#7157,1.);
#1896=VECTOR('',#7160,1.);
#1897=VECTOR('',#7171,1.);
#1898=VECTOR('',#7174,1.);
#1899=VECTOR('',#7191,0.225);
#1900=VECTOR('',#7196,0.225);
#1901=VECTOR('',#7201,0.225);
#1902=VECTOR('',#7206,0.225);
#1903=VECTOR('',#7211,1.49);
#1904=VECTOR('',#7220,0.71);
#1905=VECTOR('',#7223,2.);
#1906=VECTOR('',#7232,1.);
#1907=VECTOR('',#7235,1.);
#1908=VECTOR('',#7256,1.);
#1909=VECTOR('',#7259,1.);
#1910=VECTOR('',#7270,1.);
#1911=VECTOR('',#7273,1.);
#1912=VECTOR('',#7284,1.);
#1913=VECTOR('',#7287,1.);
#1914=VECTOR('',#7304,0.225);
#1915=VECTOR('',#7309,0.225);
#1916=VECTOR('',#7314,0.225);
#1917=VECTOR('',#7319,0.225);
#1918=VECTOR('',#7324,1.49);
#1919=VECTOR('',#7333,0.71);
#1920=VECTOR('',#7336,2.);
#1921=VECTOR('',#7351,0.4);
#1922=VECTOR('',#7356,0.425);
#1923=VECTOR('',#7361,0.41);
#1924=VECTOR('',#7370,0.26);
#1925=VECTOR('',#7375,0.25);
#1926=VECTOR('',#7380,0.225);
#1927=VECTOR('',#7385,1.);
#1928=VECTOR('',#7386,1.);
#1929=VECTOR('',#7387,1.);
#1930=VECTOR('',#7388,1.);
#1931=VECTOR('',#7391,1.);
#1932=VECTOR('',#7392,1.);
#1933=VECTOR('',#7393,1.);
#1934=VECTOR('',#7396,1.);
#1935=VECTOR('',#7397,1.);
#1936=VECTOR('',#7398,1.);
#1937=VECTOR('',#7401,1.);
#1938=VECTOR('',#7402,1.);
#1939=VECTOR('',#7403,1.);
#1940=VECTOR('',#7406,1.);
#1941=VECTOR('',#7407,1.);
#1942=VECTOR('',#7408,1.);
#1943=VECTOR('',#7411,1.);
#1944=VECTOR('',#7412,1.);
#1945=VECTOR('',#7435,0.976185);
#1946=VECTOR('',#7442,0.5);
#1947=VECTOR('',#7447,0.53);
#1948=VECTOR('',#7456,0.976185);
#1949=VECTOR('',#7463,0.53);
#1950=VECTOR('',#7482,1.023815);
#1951=VECTOR('',#7493,1.47);
#1952=VECTOR('',#7498,1.5);
#1953=VECTOR('',#7503,1.47);
#1954=VECTOR('',#7508,1.023815);
#1955=VECTOR('',#7559,1.019052);
#1956=VECTOR('',#7636,0.980948);
#1957=VECTOR('',#7665,1.013815);
#1958=VECTOR('',#7672,0.991185);
#1959=VECTOR('',#7683,1.013815);
#1960=VECTOR('',#7690,0.991185);
#1961=VECTOR('',#7709,0.165);
#1962=VECTOR('',#7718,0.25);
#1963=VECTOR('',#7723,1.);
#1964=VECTOR('',#7726,1.);
#1965=VECTOR('',#7731,1.);
#1966=VECTOR('',#7734,1.);
#1967=VECTOR('',#7735,1.);
#1968=VECTOR('',#7736,1.);
#1969=VECTOR('',#7739,1.);
#1970=VECTOR('',#7744,1.);
#1971=VECTOR('',#7745,1.);
#1972=VECTOR('',#7748,1.);
#1973=VECTOR('',#7749,1.);
#1974=VECTOR('',#7752,1.);
#1975=VECTOR('',#7753,1.);
#1976=VECTOR('',#7754,1.);
#1977=VECTOR('',#7757,1.);
#1978=VECTOR('',#7758,1.);
#1979=VECTOR('',#7759,1.);
#1980=VECTOR('',#7762,1.);
#1981=VECTOR('',#7783,0.7);
#1982=VECTOR('',#7786,0.5);
#1983=VECTOR('',#7793,0.5);
#1984=VECTOR('',#7804,0.505);
#1985=VECTOR('',#7811,0.7);
#1986=VECTOR('',#7822,1.);
#1987=VECTOR('',#7829,0.165);
#1988=VECTOR('',#7834,1.);
#1989=VECTOR('',#7837,1.);
#1990=VECTOR('',#7842,0.165);
#1991=VECTOR('',#7847,1.);
#1992=VECTOR('',#7852,0.505);
#1993=VECTOR('',#7853,0.505);
#1994=VECTOR('',#7860,0.9);
#1995=VECTOR('',#7861,0.9);
#1996=VECTOR('',#7884,0.5);
#1997=VECTOR('',#7887,0.3);
#1998=VECTOR('',#7894,0.3);
#1999=VECTOR('',#7905,0.5);
#2000=VECTOR('',#7910,1.);
#2001=VECTOR('',#7913,1.);
#2002=VECTOR('',#7918,1.);
#2003=VECTOR('',#7921,1.);
#2004=VECTOR('',#7924,1.);
#2005=VECTOR('',#7925,1.);
#2006=VECTOR('',#7928,1.);
#2007=VECTOR('',#7929,1.);
#2008=VECTOR('',#7942,0.505);
#2009=VECTOR('',#7949,0.7);
#2010=VECTOR('',#7962,0.225);
#2011=VECTOR('',#7969,0.7);
#2012=VECTOR('',#7982,0.4);
#2013=VECTOR('',#7989,1.4);
#2014=VECTOR('',#8000,1.);
#2015=VECTOR('',#8001,1.);
#2016=VECTOR('',#8002,1.);
#2017=VECTOR('',#8003,1.);
#2018=VECTOR('',#8006,1.);
#2019=VECTOR('',#8007,1.);
#2020=VECTOR('',#8008,1.);
#2021=VECTOR('',#8011,1.);
#2022=VECTOR('',#8012,1.);
#2023=VECTOR('',#8013,1.);
#2024=VECTOR('',#8016,1.);
#2025=VECTOR('',#8017,1.);
#2026=VECTOR('',#8018,1.);
#2027=VECTOR('',#8021,1.);
#2028=VECTOR('',#8022,1.);
#2029=VECTOR('',#8023,1.);
#2030=VECTOR('',#8026,1.);
#2031=VECTOR('',#8027,1.);
#2032=VECTOR('',#8044,0.325);
#2033=VECTOR('',#8049,0.35);
#2034=VECTOR('',#8054,0.335);
#2035=VECTOR('',#8063,0.21);
#2036=VECTOR('',#8066,0.2);
#2037=VECTOR('',#8115,0.165);
#2038=VECTOR('',#8122,0.165);
#2039=VECTOR('',#8129,0.165);
#2040=VECTOR('',#8136,0.165);
#2041=VECTOR('',#8143,1.);
#2042=VECTOR('',#8146,1.);
#2043=VECTOR('',#8151,1.);
#2044=VECTOR('',#8154,1.);
#2045=VECTOR('',#8159,1.);
#2046=VECTOR('',#8162,1.);
#2047=VECTOR('',#8165,1.);
#2048=VECTOR('',#8168,1.);
#2049=VECTOR('',#8175,1.);
#2050=VECTOR('',#8182,1.);
#2051=VECTOR('',#8189,1.);
#2052=VECTOR('',#8194,1.);
#2053=VECTOR('',#8195,1.);
#2054=VECTOR('',#8196,1.);
#2055=VECTOR('',#8199,1.);
#2056=VECTOR('',#8200,1.);
#2057=VECTOR('',#8201,1.);
#2058=VECTOR('',#8206,1.);
#2059=VECTOR('',#8207,1.);
#2060=VECTOR('',#8208,1.);
#2061=VECTOR('',#8211,1.);
#2062=VECTOR('',#8212,1.);
#2063=VECTOR('',#8213,1.);
#2064=VECTOR('',#8216,1.);
#2065=VECTOR('',#8217,1.);
#2066=VECTOR('',#8218,1.);
#2067=VECTOR('',#8221,1.);
#2068=VECTOR('',#8222,1.);
#2069=VECTOR('',#8223,1.);
#2070=VECTOR('',#8226,1.);
#2071=VECTOR('',#8227,1.);
#2072=VECTOR('',#8228,1.);
#2073=VECTOR('',#8231,1.);
#2074=VECTOR('',#8232,1.);
#2075=VECTOR('',#8233,1.);
#2076=VECTOR('',#8240,1.);
#2077=VECTOR('',#8243,1.);
#2078=VECTOR('',#8248,1.);
#2079=VECTOR('',#8249,1.);
#2080=VECTOR('',#8252,1.);
#2081=VECTOR('',#8253,1.);
#2082=VECTOR('',#8256,1.);
#2083=VECTOR('',#8257,1.);
#2084=VECTOR('',#8258,1.);
#2085=VECTOR('',#8261,1.);
#2086=VECTOR('',#8264,1.);
#2087=VECTOR('',#8265,1.);
#2088=VECTOR('',#8270,1.);
#2089=VECTOR('',#8271,1.);
#2090=VECTOR('',#8272,1.);
#2091=VECTOR('',#8281,1.);
#2092=VECTOR('',#8288,1.);
#2093=VECTOR('',#8289,1.);
#2094=VECTOR('',#8290,1.);
#2095=VECTOR('',#8299,1.);
#2096=VECTOR('',#8300,1.);
#2097=VECTOR('',#8301,1.);
#2098=VECTOR('',#8304,1.);
#2099=VECTOR('',#8307,0.7);
#2100=VECTOR('',#8312,1.);
#2101=VECTOR('',#8315,1.);
#2102=VECTOR('',#8318,1.);
#2103=VECTOR('',#8321,1.);
#2104=VECTOR('',#8324,1.);
#2105=VECTOR('',#8329,1.);
#2106=VECTOR('',#8332,1.);
#2107=VECTOR('',#8335,1.);
#2108=VECTOR('',#8338,1.);
#2109=VECTOR('',#8339,1.);
#2110=VECTOR('',#8340,1.);
#2111=VECTOR('',#8343,1.);
#2112=VECTOR('',#8346,1.);
#2113=VECTOR('',#8347,1.);
#2114=VECTOR('',#8352,1.);
#2115=VECTOR('',#8353,1.);
#2116=VECTOR('',#8354,1.);
#2117=VECTOR('',#8365,1.);
#2118=VECTOR('',#8370,1.);
#2119=VECTOR('',#8373,1.);
#2120=VECTOR('',#8376,1.);
#2121=VECTOR('',#8379,1.);
#2122=VECTOR('',#8380,1.);
#2123=VECTOR('',#8381,1.);
#2124=VECTOR('',#8384,1.);
#2125=VECTOR('',#8387,1.);
#2126=VECTOR('',#8388,1.);
#2127=VECTOR('',#8393,1.);
#2128=VECTOR('',#8394,1.);
#2129=VECTOR('',#8395,1.);
#2130=VECTOR('',#8406,1.);
#2131=VECTOR('',#8411,1.);
#2132=VECTOR('',#8414,1.);
#2133=VECTOR('',#8417,1.);
#2134=VECTOR('',#8420,1.);
#2135=VECTOR('',#8423,1.);
#2136=VECTOR('',#8430,1.);
#2137=VECTOR('',#8431,1.);
#2138=VECTOR('',#8442,0.5);
#2139=VECTOR('',#8453,0.505);
#2140=VECTOR('',#8460,0.7);
#2141=VECTOR('',#8471,1.);
#2142=VECTOR('',#8478,0.165);
#2143=VECTOR('',#8483,1.);
#2144=VECTOR('',#8486,1.);
#2145=VECTOR('',#8491,0.165);
#2146=VECTOR('',#8496,1.);
#2147=VECTOR('',#8501,0.505);
#2148=VECTOR('',#8502,0.505);
#2149=VECTOR('',#8509,0.9);
#2150=VECTOR('',#8510,0.9);
#2151=VECTOR('',#8525,1.);
#2152=VECTOR('',#8526,1.);
#2153=VECTOR('',#8527,1.);
#2154=VECTOR('',#8528,1.);
#2155=VECTOR('',#8531,1.);
#2156=VECTOR('',#8532,1.);
#2157=VECTOR('',#8533,1.);
#2158=VECTOR('',#8536,1.);
#2159=VECTOR('',#8537,1.);
#2160=VECTOR('',#8538,1.);
#2161=VECTOR('',#8541,1.);
#2162=VECTOR('',#8542,1.);
#2163=VECTOR('',#8543,1.);
#2164=VECTOR('',#8546,1.);
#2165=VECTOR('',#8547,1.);
#2166=VECTOR('',#8548,1.);
#2167=VECTOR('',#8551,1.);
#2168=VECTOR('',#8552,1.);
#2169=VECTOR('',#8563,0.185);
#2170=VECTOR('',#8566,0.2);
#2171=CIRCLE('',#6014,0.21);
#2172=CIRCLE('',#6015,0.21);
#2173=CIRCLE('',#6017,0.21);
#2174=CIRCLE('',#6018,0.21);
#2175=CIRCLE('',#6020,0.21);
#2176=CIRCLE('',#6021,0.21);
#2177=CIRCLE('',#6023,0.21);
#2178=CIRCLE('',#6024,0.21);
#2179=CIRCLE('',#6047,0.25);
#2180=CIRCLE('',#6049,0.165);
#2181=CIRCLE('',#6050,0.165);
#2182=CIRCLE('',#6053,0.165);
#2183=CIRCLE('',#6054,0.165);
#2184=CIRCLE('',#6057,0.165);
#2185=CIRCLE('',#6058,0.165);
#2186=CIRCLE('',#6061,0.165);
#2187=CIRCLE('',#6062,0.165);
#2188=CIRCLE('',#6065,1.5);
#2189=CIRCLE('',#6066,1.5);
#2190=CIRCLE('',#6068,1.02);
#2191=CIRCLE('',#6070,1.02);
#2192=CIRCLE('',#6072,0.25);
#2193=CIRCLE('',#6074,0.165);
#2194=CIRCLE('',#6075,0.165);
#2195=CIRCLE('',#6078,0.165);
#2196=CIRCLE('',#6079,0.165);
#2197=CIRCLE('',#6082,0.165);
#2198=CIRCLE('',#6083,0.165);
#2199=CIRCLE('',#6086,0.165);
#2200=CIRCLE('',#6087,0.165);
#2201=CIRCLE('',#6090,1.5);
#2202=CIRCLE('',#6091,1.5);
#2203=CIRCLE('',#6093,1.02);
#2204=CIRCLE('',#6095,1.02);
#2205=CIRCLE('',#6097,0.5);
#2206=CIRCLE('',#6098,0.5);
#2207=CIRCLE('',#6100,0.5);
#2208=CIRCLE('',#6101,0.5);
#2209=CIRCLE('',#6103,0.275);
#2210=CIRCLE('',#6105,0.5);
#2211=CIRCLE('',#6106,0.5);
#2212=CIRCLE('',#6108,0.5);
#2213=CIRCLE('',#6109,0.5);
#2214=CIRCLE('',#6111,0.275);
#2215=CIRCLE('',#6113,0.5);
#2216=CIRCLE('',#6114,0.5);
#2217=CIRCLE('',#6116,0.5);
#2218=CIRCLE('',#6117,0.5);
#2219=CIRCLE('',#6119,0.275);
#2220=CIRCLE('',#6121,0.5);
#2221=CIRCLE('',#6122,0.5);
#2222=CIRCLE('',#6124,0.5);
#2223=CIRCLE('',#6125,0.5);
#2224=CIRCLE('',#6127,0.275);
#2225=CIRCLE('',#6134,0.275);
#2226=CIRCLE('',#6136,0.275);
#2227=CIRCLE('',#6138,0.275);
#2228=CIRCLE('',#6140,0.275);
#2229=CIRCLE('',#6148,0.375);
#2230=CIRCLE('',#6149,0.375);
#2231=CIRCLE('',#6151,2.);
#2232=CIRCLE('',#6152,2.);
#2233=CIRCLE('',#6153,0.225);
#2234=CIRCLE('',#6155,2.);
#2235=CIRCLE('',#6156,0.375);
#2236=CIRCLE('',#6157,0.225);
#2237=CIRCLE('',#6159,0.375);
#2238=CIRCLE('',#6161,2.);
#2239=CIRCLE('',#6162,0.375);
#2240=CIRCLE('',#6163,0.225);
#2241=CIRCLE('',#6165,0.375);
#2242=CIRCLE('',#6167,2.);
#2243=CIRCLE('',#6168,0.375);
#2244=CIRCLE('',#6169,0.225);
#2245=CIRCLE('',#6171,0.375);
#2246=CIRCLE('',#6173,2.);
#2247=CIRCLE('',#6174,2.);
#2248=CIRCLE('',#6175,2.);
#2249=CIRCLE('',#6176,2.);
#2250=CIRCLE('',#6177,0.71);
#2251=CIRCLE('',#6179,0.225);
#2252=CIRCLE('',#6181,0.225);
#2253=CIRCLE('',#6183,0.225);
#2254=CIRCLE('',#6185,0.225);
#2255=CIRCLE('',#6187,1.49);
#2256=CIRCLE('',#6188,1.49);
#2257=CIRCLE('',#6190,0.71);
#2258=CIRCLE('',#6193,2.);
#2259=CIRCLE('',#6197,0.375);
#2260=CIRCLE('',#6198,0.375);
#2261=CIRCLE('',#6200,2.);
#2262=CIRCLE('',#6201,2.);
#2263=CIRCLE('',#6202,0.225);
#2264=CIRCLE('',#6204,2.);
#2265=CIRCLE('',#6205,0.375);
#2266=CIRCLE('',#6206,0.225);
#2267=CIRCLE('',#6208,0.375);
#2268=CIRCLE('',#6210,2.);
#2269=CIRCLE('',#6211,0.375);
#2270=CIRCLE('',#6212,0.225);
#2271=CIRCLE('',#6214,0.375);
#2272=CIRCLE('',#6216,2.);
#2273=CIRCLE('',#6217,0.375);
#2274=CIRCLE('',#6218,0.225);
#2275=CIRCLE('',#6220,0.375);
#2276=CIRCLE('',#6222,2.);
#2277=CIRCLE('',#6223,2.);
#2278=CIRCLE('',#6224,2.);
#2279=CIRCLE('',#6225,2.);
#2280=CIRCLE('',#6226,0.71);
#2281=CIRCLE('',#6228,0.225);
#2282=CIRCLE('',#6230,0.225);
#2283=CIRCLE('',#6232,0.225);
#2284=CIRCLE('',#6234,0.225);
#2285=CIRCLE('',#6236,1.49);
#2286=CIRCLE('',#6237,1.49);
#2287=CIRCLE('',#6239,0.71);
#2288=CIRCLE('',#6242,2.);
#2289=CIRCLE('',#6246,0.375);
#2290=CIRCLE('',#6248,0.425);
#2291=CIRCLE('',#6250,0.425);
#2292=CIRCLE('',#6252,0.395);
#2293=CIRCLE('',#6254,0.27);
#2294=CIRCLE('',#6256,0.24505);
#2295=CIRCLE('',#6258,0.24505);
#2296=CIRCLE('',#6260,0.2);
#2297=CIRCLE('',#6273,0.976185);
#2298=CIRCLE('',#6274,0.976185);
#2299=CIRCLE('',#6275,0.247676);
#2300=CIRCLE('',#6276,0.976185);
#2301=CIRCLE('',#6277,0.976185);
#2302=CIRCLE('',#6279,0.976185);
#2303=CIRCLE('',#6281,0.5);
#2304=CIRCLE('',#6282,0.5);
#2305=CIRCLE('',#6284,0.56);
#2306=CIRCLE('',#6287,0.976185);
#2307=CIRCLE('',#6289,0.56);
#2308=CIRCLE('',#6293,1.023815);
#2309=CIRCLE('',#6294,1.023815);
#2310=CIRCLE('',#6295,0.247676);
#2311=CIRCLE('',#6296,1.023815);
#2312=CIRCLE('',#6297,1.023815);
#2313=CIRCLE('',#6299,1.023815);
#2314=CIRCLE('',#6301,1.44);
#2315=CIRCLE('',#6302,1.023815);
#2316=CIRCLE('',#6304,1.5);
#2317=CIRCLE('',#6306,1.5);
#2318=CIRCLE('',#6308,1.44);
#2319=CIRCLE('',#6313,0.23815);
#2320=CIRCLE('',#6315,0.23815);
#2321=CIRCLE('',#6317,0.23815);
#2322=CIRCLE('',#6319,0.23815);
#2323=CIRCLE('',#6321,0.23815);
#2324=CIRCLE('',#6323,0.23815);
#2325=CIRCLE('',#6325,0.23815);
#2326=CIRCLE('',#6327,0.23815);
#2327=CIRCLE('',#6330,0.243053047864041);
#2328=CIRCLE('',#6331,0.243053047864041);
#2329=CIRCLE('',#6333,1.019052);
#2330=CIRCLE('',#6334,1.019052);
#2331=CIRCLE('',#6335,1.019052);
#2332=CIRCLE('',#6336,1.019052);
#2333=CIRCLE('',#6337,1.019052);
#2334=CIRCLE('',#6338,1.019052);
#2335=CIRCLE('',#6339,1.019052);
#2336=CIRCLE('',#6340,1.019052);
#2337=CIRCLE('',#6341,1.019052);
#2338=CIRCLE('',#6343,0.980948);
#2339=CIRCLE('',#6344,0.243053047864041);
#2340=CIRCLE('',#6346,0.243053047864041);
#2341=CIRCLE('',#6348,0.980948);
#2342=CIRCLE('',#6349,0.243053047864041);
#2343=CIRCLE('',#6351,0.243053047864041);
#2344=CIRCLE('',#6353,0.980948);
#2345=CIRCLE('',#6354,0.243053047864041);
#2346=CIRCLE('',#6356,0.243053047864041);
#2347=CIRCLE('',#6358,0.980948);
#2348=CIRCLE('',#6359,0.243053047864041);
#2349=CIRCLE('',#6361,0.243053047864041);
#2350=CIRCLE('',#6363,0.980948);
#2351=CIRCLE('',#6364,0.243053047864041);
#2352=CIRCLE('',#6366,0.243053047864041);
#2353=CIRCLE('',#6368,0.980948);
#2354=CIRCLE('',#6369,0.243053047864041);
#2355=CIRCLE('',#6371,0.243053047864041);
#2356=CIRCLE('',#6373,0.980948);
#2357=CIRCLE('',#6374,0.980948);
#2358=CIRCLE('',#6375,0.980948);
#2359=CIRCLE('',#6377,0.243053047864041);
#2360=CIRCLE('',#6379,0.243053047864041);
#2361=CIRCLE('',#6384,1.013815);
#2362=CIRCLE('',#6385,0.991185);
#2363=CIRCLE('',#6387,1.013815);
#2364=CIRCLE('',#6389,0.991185);
#2365=CIRCLE('',#6392,1.013815);
#2366=CIRCLE('',#6393,0.991185);
#2367=CIRCLE('',#6395,1.013815);
#2368=CIRCLE('',#6397,0.991185);
#2369=CIRCLE('',#6407,0.165);
#2370=CIRCLE('',#6408,0.165);
#2371=CIRCLE('',#6411,0.25);
#2372=CIRCLE('',#6412,0.25);
#2373=CIRCLE('',#6414,0.5);
#2374=CIRCLE('',#6415,0.5);
#2375=CIRCLE('',#6417,1.);
#2376=CIRCLE('',#6418,1.);
#2377=CIRCLE('',#6419,0.7);
#2378=CIRCLE('',#6426,1.);
#2379=CIRCLE('',#6427,1.);
#2380=CIRCLE('',#6428,0.5);
#2381=CIRCLE('',#6432,0.7);
#2382=CIRCLE('',#6433,0.5);
#2383=CIRCLE('',#6436,0.5);
#2384=CIRCLE('',#6438,0.5);
#2385=CIRCLE('',#6443,0.505);
#2386=CIRCLE('',#6444,0.505);
#2387=CIRCLE('',#6446,0.7);
#2388=CIRCLE('',#6447,0.7);
#2389=CIRCLE('',#6452,0.165);
#2390=CIRCLE('',#6453,0.165);
#2391=CIRCLE('',#6455,0.165);
#2392=CIRCLE('',#6458,0.165);
#2393=CIRCLE('',#6460,0.165);
#2394=CIRCLE('',#6463,0.505);
#2395=CIRCLE('',#6464,0.505);
#2396=CIRCLE('',#6466,0.9);
#2397=CIRCLE('',#6467,0.9);
#2398=CIRCLE('',#6472,0.5);
#2399=CIRCLE('',#6473,0.3);
#2400=CIRCLE('',#6475,0.5);
#2401=CIRCLE('',#6476,0.3);
#2402=CIRCLE('',#6479,0.3);
#2403=CIRCLE('',#6481,0.3);
#2404=CIRCLE('',#6486,0.5);
#2405=CIRCLE('',#6487,0.5);
#2406=CIRCLE('',#6489,0.6);
#2407=CIRCLE('',#6490,0.6);
#2408=CIRCLE('',#6492,1.8);
#2409=CIRCLE('',#6496,1.8);
#2410=CIRCLE('',#6500,0.505);
#2411=CIRCLE('',#6501,0.505);
#2412=CIRCLE('',#6503,0.7);
#2413=CIRCLE('',#6504,0.7);
#2414=CIRCLE('',#6509,0.225);
#2415=CIRCLE('',#6510,0.225);
#2416=CIRCLE('',#6512,0.7);
#2417=CIRCLE('',#6513,0.7);
#2418=CIRCLE('',#6518,0.4);
#2419=CIRCLE('',#6519,0.4);
#2420=CIRCLE('',#6521,1.4);
#2421=CIRCLE('',#6522,1.4);
#2422=CIRCLE('',#6535,0.1954);
#2423=CIRCLE('',#6537,0.3);
#2424=CIRCLE('',#6539,0.35);
#2425=CIRCLE('',#6541,0.35);
#2426=CIRCLE('',#6543,0.32);
#2427=CIRCLE('',#6545,0.22);
#2428=CIRCLE('',#6547,0.1954);
#2429=CIRCLE('',#6572,0.165);
#2430=CIRCLE('',#6573,0.165);
#2431=CIRCLE('',#6575,0.165);
#2432=CIRCLE('',#6576,0.165);
#2433=CIRCLE('',#6578,0.165);
#2434=CIRCLE('',#6579,0.165);
#2435=CIRCLE('',#6581,0.165);
#2436=CIRCLE('',#6582,0.165);
#2437=CIRCLE('',#6584,1.82);
#2438=CIRCLE('',#6585,1.82);
#2439=CIRCLE('',#6587,1.82);
#2440=CIRCLE('',#6588,1.82);
#2441=CIRCLE('',#6590,1.82);
#2442=CIRCLE('',#6591,1.82);
#2443=CIRCLE('',#6593,1.82);
#2444=CIRCLE('',#6594,1.82);
#2445=CIRCLE('',#6596,3.);
#2446=CIRCLE('',#6597,3.);
#2447=CIRCLE('',#6599,3.);
#2448=CIRCLE('',#6600,3.);
#2449=CIRCLE('',#6602,3.);
#2450=CIRCLE('',#6603,3.);
#2451=CIRCLE('',#6605,0.32);
#2452=CIRCLE('',#6606,3.);
#2453=CIRCLE('',#6607,3.);
#2454=CIRCLE('',#6608,0.32);
#2455=CIRCLE('',#6609,3.);
#2456=CIRCLE('',#6610,0.32);
#2457=CIRCLE('',#6611,3.);
#2458=CIRCLE('',#6612,0.32);
#2459=CIRCLE('',#6613,3.);
#2460=CIRCLE('',#6615,3.);
#2461=CIRCLE('',#6617,3.);
#2462=CIRCLE('',#6624,3.);
#2463=CIRCLE('',#6625,0.32);
#2464=CIRCLE('',#6626,0.7);
#2465=CIRCLE('',#6627,0.32);
#2466=CIRCLE('',#6629,0.32);
#2467=CIRCLE('',#6630,0.7);
#2468=CIRCLE('',#6631,0.32);
#2469=CIRCLE('',#6633,0.7);
#2470=CIRCLE('',#6634,0.32);
#2471=CIRCLE('',#6637,0.7);
#2472=CIRCLE('',#6638,0.7);
#2473=CIRCLE('',#6639,0.7);
#2474=CIRCLE('',#6640,0.7);
#2475=CIRCLE('',#6641,0.7);
#2476=CIRCLE('',#6642,0.7);
#2477=CIRCLE('',#6643,0.7);
#2478=CIRCLE('',#6652,3.);
#2479=CIRCLE('',#6653,0.32);
#2480=CIRCLE('',#6654,0.32);
#2481=CIRCLE('',#6656,0.32);
#2482=CIRCLE('',#6666,3.);
#2483=CIRCLE('',#6667,0.32);
#2484=CIRCLE('',#6668,0.32);
#2485=CIRCLE('',#6670,0.32);
#2486=CIRCLE('',#6679,0.32);
#2487=CIRCLE('',#6684,0.5);
#2488=CIRCLE('',#6686,0.5);
#2489=CIRCLE('',#6690,0.505);
#2490=CIRCLE('',#6691,0.505);
#2491=CIRCLE('',#6693,0.7);
#2492=CIRCLE('',#6694,0.7);
#2493=CIRCLE('',#6699,0.165);
#2494=CIRCLE('',#6700,0.165);
#2495=CIRCLE('',#6702,0.165);
#2496=CIRCLE('',#6705,0.165);
#2497=CIRCLE('',#6707,0.165);
#2498=CIRCLE('',#6710,0.505);
#2499=CIRCLE('',#6711,0.505);
#2500=CIRCLE('',#6713,0.9);
#2501=CIRCLE('',#6714,0.9);
#2502=CIRCLE('',#6719,0.1954);
#2503=CIRCLE('',#6728,0.17);
#2504=CIRCLE('',#6730,0.1954);
#2505=VERTEX_POINT('',#8605);
#2506=VERTEX_POINT('',#8607);
#2507=VERTEX_POINT('',#8611);
#2508=VERTEX_POINT('',#8613);
#2509=VERTEX_POINT('',#8617);
#2510=VERTEX_POINT('',#8619);
#2511=VERTEX_POINT('',#8623);
#2512=VERTEX_POINT('',#8625);
#2513=VERTEX_POINT('',#8629);
#2514=VERTEX_POINT('',#8630);
#2515=VERTEX_POINT('',#8632);
#2516=VERTEX_POINT('',#8634);
#2517=VERTEX_POINT('',#8638);
#2518=VERTEX_POINT('',#8640);
#2519=VERTEX_POINT('',#8644);
#2520=VERTEX_POINT('',#8646);
#2521=VERTEX_POINT('',#8656);
#2522=VERTEX_POINT('',#8657);
#2523=VERTEX_POINT('',#8659);
#2524=VERTEX_POINT('',#8661);
#2525=VERTEX_POINT('',#8665);
#2526=VERTEX_POINT('',#8667);
#2527=VERTEX_POINT('',#8671);
#2528=VERTEX_POINT('',#8673);
#2529=VERTEX_POINT('',#8683);
#2530=VERTEX_POINT('',#8684);
#2531=VERTEX_POINT('',#8686);
#2532=VERTEX_POINT('',#8688);
#2533=VERTEX_POINT('',#8692);
#2534=VERTEX_POINT('',#8694);
#2535=VERTEX_POINT('',#8698);
#2536=VERTEX_POINT('',#8700);
#2537=VERTEX_POINT('',#8710);
#2538=VERTEX_POINT('',#8712);
#2539=VERTEX_POINT('',#8749);
#2540=VERTEX_POINT('',#8751);
#2541=VERTEX_POINT('',#8756);
#2542=VERTEX_POINT('',#8758);
#2543=VERTEX_POINT('',#8763);
#2544=VERTEX_POINT('',#8765);
#2545=VERTEX_POINT('',#8770);
#2546=VERTEX_POINT('',#8772);
#2547=VERTEX_POINT('',#8777);
#2548=VERTEX_POINT('',#8779);
#2549=VERTEX_POINT('',#8783);
#2550=VERTEX_POINT('',#8786);
#2551=VERTEX_POINT('',#8790);
#2552=VERTEX_POINT('',#8792);
#2553=VERTEX_POINT('',#8829);
#2554=VERTEX_POINT('',#8831);
#2555=VERTEX_POINT('',#8836);
#2556=VERTEX_POINT('',#8838);
#2557=VERTEX_POINT('',#8843);
#2558=VERTEX_POINT('',#8845);
#2559=VERTEX_POINT('',#8850);
#2560=VERTEX_POINT('',#8852);
#2561=VERTEX_POINT('',#8857);
#2562=VERTEX_POINT('',#8859);
#2563=VERTEX_POINT('',#8863);
#2564=VERTEX_POINT('',#8866);
#2565=VERTEX_POINT('',#8870);
#2566=VERTEX_POINT('',#8871);
#2567=VERTEX_POINT('',#8873);
#2568=VERTEX_POINT('',#8875);
#2569=VERTEX_POINT('',#8884);
#2570=VERTEX_POINT('',#8887);
#2571=VERTEX_POINT('',#8888);
#2572=VERTEX_POINT('',#8890);
#2573=VERTEX_POINT('',#8892);
#2574=VERTEX_POINT('',#8901);
#2575=VERTEX_POINT('',#8904);
#2576=VERTEX_POINT('',#8905);
#2577=VERTEX_POINT('',#8907);
#2578=VERTEX_POINT('',#8909);
#2579=VERTEX_POINT('',#8918);
#2580=VERTEX_POINT('',#8921);
#2581=VERTEX_POINT('',#8922);
#2582=VERTEX_POINT('',#8924);
#2583=VERTEX_POINT('',#8926);
#2584=VERTEX_POINT('',#8935);
#2585=VERTEX_POINT('',#8938);
#2586=VERTEX_POINT('',#8942);
#2587=VERTEX_POINT('',#8946);
#2588=VERTEX_POINT('',#8955);
#2589=VERTEX_POINT('',#8959);
#2590=VERTEX_POINT('',#8963);
#2591=VERTEX_POINT('',#8967);
#2592=VERTEX_POINT('',#8971);
#2593=VERTEX_POINT('',#8975);
#2594=VERTEX_POINT('',#8976);
#2595=VERTEX_POINT('',#8981);
#2596=VERTEX_POINT('',#8985);
#2597=VERTEX_POINT('',#8993);
#2598=VERTEX_POINT('',#8994);
#2599=VERTEX_POINT('',#8996);
#2600=VERTEX_POINT('',#8998);
#2601=VERTEX_POINT('',#9002);
#2602=VERTEX_POINT('',#9005);
#2603=VERTEX_POINT('',#9008);
#2604=VERTEX_POINT('',#9009);
#2605=VERTEX_POINT('',#9012);
#2606=VERTEX_POINT('',#9015);
#2607=VERTEX_POINT('',#9017);
#2608=VERTEX_POINT('',#9021);
#2609=VERTEX_POINT('',#9022);
#2610=VERTEX_POINT('',#9025);
#2611=VERTEX_POINT('',#9028);
#2612=VERTEX_POINT('',#9030);
#2613=VERTEX_POINT('',#9034);
#2614=VERTEX_POINT('',#9035);
#2615=VERTEX_POINT('',#9038);
#2616=VERTEX_POINT('',#9041);
#2617=VERTEX_POINT('',#9043);
#2618=VERTEX_POINT('',#9051);
#2619=VERTEX_POINT('',#9054);
#2620=VERTEX_POINT('',#9058);
#2621=VERTEX_POINT('',#9062);
#2622=VERTEX_POINT('',#9066);
#2623=VERTEX_POINT('',#9070);
#2624=VERTEX_POINT('',#9072);
#2625=VERTEX_POINT('',#9076);
#2626=VERTEX_POINT('',#9081);
#2627=VERTEX_POINT('',#9087);
#2628=VERTEX_POINT('',#9088);
#2629=VERTEX_POINT('',#9090);
#2630=VERTEX_POINT('',#9092);
#2631=VERTEX_POINT('',#9096);
#2632=VERTEX_POINT('',#9099);
#2633=VERTEX_POINT('',#9102);
#2634=VERTEX_POINT('',#9103);
#2635=VERTEX_POINT('',#9106);
#2636=VERTEX_POINT('',#9109);
#2637=VERTEX_POINT('',#9111);
#2638=VERTEX_POINT('',#9115);
#2639=VERTEX_POINT('',#9116);
#2640=VERTEX_POINT('',#9119);
#2641=VERTEX_POINT('',#9122);
#2642=VERTEX_POINT('',#9124);
#2643=VERTEX_POINT('',#9128);
#2644=VERTEX_POINT('',#9129);
#2645=VERTEX_POINT('',#9132);
#2646=VERTEX_POINT('',#9135);
#2647=VERTEX_POINT('',#9137);
#2648=VERTEX_POINT('',#9145);
#2649=VERTEX_POINT('',#9148);
#2650=VERTEX_POINT('',#9152);
#2651=VERTEX_POINT('',#9156);
#2652=VERTEX_POINT('',#9160);
#2653=VERTEX_POINT('',#9164);
#2654=VERTEX_POINT('',#9166);
#2655=VERTEX_POINT('',#9170);
#2656=VERTEX_POINT('',#9175);
#2657=VERTEX_POINT('',#9181);
#2658=VERTEX_POINT('',#9184);
#2659=VERTEX_POINT('',#9188);
#2660=VERTEX_POINT('',#9192);
#2661=VERTEX_POINT('',#9196);
#2662=VERTEX_POINT('',#9199);
#2663=VERTEX_POINT('',#9203);
#2664=VERTEX_POINT('',#9207);
#2665=VERTEX_POINT('',#9212);
#2666=VERTEX_POINT('',#9213);
#2667=VERTEX_POINT('',#9215);
#2668=VERTEX_POINT('',#9217);
#2669=VERTEX_POINT('',#9221);
#2670=VERTEX_POINT('',#9223);
#2671=VERTEX_POINT('',#9227);
#2672=VERTEX_POINT('',#9229);
#2673=VERTEX_POINT('',#9233);
#2674=VERTEX_POINT('',#9235);
#2675=VERTEX_POINT('',#9239);
#2676=VERTEX_POINT('',#9241);
#2677=VERTEX_POINT('',#9252);
#2678=VERTEX_POINT('',#9253);
#2679=VERTEX_POINT('',#9256);
#2680=VERTEX_POINT('',#9258);
#2681=VERTEX_POINT('',#9262);
#2682=VERTEX_POINT('',#9266);
#2683=VERTEX_POINT('',#9268);
#2684=VERTEX_POINT('',#9272);
#2685=VERTEX_POINT('',#9277);
#2686=VERTEX_POINT('',#9281);
#2687=VERTEX_POINT('',#9287);
#2688=VERTEX_POINT('',#9288);
#2689=VERTEX_POINT('',#9291);
#2690=VERTEX_POINT('',#9293);
#2691=VERTEX_POINT('',#9297);
#2692=VERTEX_POINT('',#9301);
#2693=VERTEX_POINT('',#9303);
#2694=VERTEX_POINT('',#9306);
#2695=VERTEX_POINT('',#9310);
#2696=VERTEX_POINT('',#9314);
#2697=VERTEX_POINT('',#9322);
#2698=VERTEX_POINT('',#9323);
#2699=VERTEX_POINT('',#9326);
#2700=VERTEX_POINT('',#9327);
#2701=VERTEX_POINT('',#9330);
#2702=VERTEX_POINT('',#9331);
#2703=VERTEX_POINT('',#9334);
#2704=VERTEX_POINT('',#9335);
#2705=VERTEX_POINT('',#9338);
#2706=VERTEX_POINT('',#9339);
#2707=VERTEX_POINT('',#9342);
#2708=VERTEX_POINT('',#9343);
#2709=VERTEX_POINT('',#9346);
#2710=VERTEX_POINT('',#9347);
#2711=VERTEX_POINT('',#9350);
#2712=VERTEX_POINT('',#9351);
#2713=VERTEX_POINT('',#9355);
#2714=VERTEX_POINT('',#9356);
#2715=VERTEX_POINT('',#9379);
#2716=VERTEX_POINT('',#9381);
#2717=VERTEX_POINT('',#9406);
#2718=VERTEX_POINT('',#9408);
#2719=VERTEX_POINT('',#9431);
#2720=VERTEX_POINT('',#9433);
#2721=VERTEX_POINT('',#9456);
#2722=VERTEX_POINT('',#9458);
#2723=VERTEX_POINT('',#9471);
#2724=VERTEX_POINT('',#9474);
#2725=VERTEX_POINT('',#9487);
#2726=VERTEX_POINT('',#9489);
#2727=VERTEX_POINT('',#9512);
#2728=VERTEX_POINT('',#9514);
#2729=VERTEX_POINT('',#9537);
#2730=VERTEX_POINT('',#9539);
#2731=VERTEX_POINT('',#9562);
#2732=VERTEX_POINT('',#9564);
#2733=VERTEX_POINT('',#9589);
#2734=VERTEX_POINT('',#9593);
#2735=VERTEX_POINT('',#9618);
#2736=VERTEX_POINT('',#9622);
#2737=VERTEX_POINT('',#9647);
#2738=VERTEX_POINT('',#9651);
#2739=VERTEX_POINT('',#9652);
#2740=VERTEX_POINT('',#9679);
#2741=VERTEX_POINT('',#9683);
#2742=VERTEX_POINT('',#9708);
#2743=VERTEX_POINT('',#9712);
#2744=VERTEX_POINT('',#9737);
#2745=VERTEX_POINT('',#9741);
#2746=VERTEX_POINT('',#9766);
#2747=VERTEX_POINT('',#9769);
#2748=VERTEX_POINT('',#9771);
#2749=VERTEX_POINT('',#9803);
#2750=VERTEX_POINT('',#9805);
#2751=VERTEX_POINT('',#9808);
#2752=VERTEX_POINT('',#9812);
#2753=VERTEX_POINT('',#9817);
#2754=VERTEX_POINT('',#9819);
#2755=VERTEX_POINT('',#9822);
#2756=VERTEX_POINT('',#9826);
#2757=VERTEX_POINT('',#9838);
#2758=VERTEX_POINT('',#9840);
#2759=VERTEX_POINT('',#9845);
#2760=VERTEX_POINT('',#9847);
#2761=VERTEX_POINT('',#9851);
#2762=VERTEX_POINT('',#9852);
#2763=VERTEX_POINT('',#9854);
#2764=VERTEX_POINT('',#9856);
#2765=VERTEX_POINT('',#9860);
#2766=VERTEX_POINT('',#9862);
#2767=VERTEX_POINT('',#9864);
#2768=VERTEX_POINT('',#9866);
#2769=VERTEX_POINT('',#9868);
#2770=VERTEX_POINT('',#9870);
#2771=VERTEX_POINT('',#9873);
#2772=VERTEX_POINT('',#9876);
#2773=VERTEX_POINT('',#9880);
#2774=VERTEX_POINT('',#9884);
#2775=VERTEX_POINT('',#9886);
#2776=VERTEX_POINT('',#9890);
#2777=VERTEX_POINT('',#9892);
#2778=VERTEX_POINT('',#9900);
#2779=VERTEX_POINT('',#9905);
#2780=VERTEX_POINT('',#9907);
#2781=VERTEX_POINT('',#9912);
#2782=VERTEX_POINT('',#9916);
#2783=VERTEX_POINT('',#9923);
#2784=VERTEX_POINT('',#9925);
#2785=VERTEX_POINT('',#9929);
#2786=VERTEX_POINT('',#9931);
#2787=VERTEX_POINT('',#9938);
#2788=VERTEX_POINT('',#9939);
#2789=VERTEX_POINT('',#9941);
#2790=VERTEX_POINT('',#9945);
#2791=VERTEX_POINT('',#9981);
#2792=VERTEX_POINT('',#9996);
#2793=VERTEX_POINT('',#10015);
#2794=VERTEX_POINT('',#10016);
#2795=VERTEX_POINT('',#10020);
#2796=VERTEX_POINT('',#10021);
#2797=VERTEX_POINT('',#10032);
#2798=VERTEX_POINT('',#10061);
#2799=VERTEX_POINT('',#10063);
#2800=VERTEX_POINT('',#10072);
#2801=VERTEX_POINT('',#10074);
#2802=VERTEX_POINT('',#10102);
#2803=VERTEX_POINT('',#10105);
#2804=VERTEX_POINT('',#10109);
#2805=VERTEX_POINT('',#10112);
#2806=VERTEX_POINT('',#10119);
#2807=VERTEX_POINT('',#10121);
#2808=VERTEX_POINT('',#10124);
#2809=VERTEX_POINT('',#10126);
#2810=VERTEX_POINT('',#10131);
#2811=VERTEX_POINT('',#10135);
#2812=VERTEX_POINT('',#10142);
#2813=VERTEX_POINT('',#10144);
#2814=VERTEX_POINT('',#10148);
#2815=VERTEX_POINT('',#10149);
#2816=VERTEX_POINT('',#10151);
#2817=VERTEX_POINT('',#10153);
#2818=VERTEX_POINT('',#10157);
#2819=VERTEX_POINT('',#10159);
#2820=VERTEX_POINT('',#10163);
#2821=VERTEX_POINT('',#10167);
#2822=VERTEX_POINT('',#10175);
#2823=VERTEX_POINT('',#10177);
#2824=VERTEX_POINT('',#10181);
#2825=VERTEX_POINT('',#10183);
#2826=VERTEX_POINT('',#10190);
#2827=VERTEX_POINT('',#10192);
#2828=VERTEX_POINT('',#10196);
#2829=VERTEX_POINT('',#10198);
#2830=VERTEX_POINT('',#10205);
#2831=VERTEX_POINT('',#10207);
#2832=VERTEX_POINT('',#10211);
#2833=VERTEX_POINT('',#10213);
#2834=VERTEX_POINT('',#10220);
#2835=VERTEX_POINT('',#10221);
#2836=VERTEX_POINT('',#10223);
#2837=VERTEX_POINT('',#10225);
#2838=VERTEX_POINT('',#10229);
#2839=VERTEX_POINT('',#10231);
#2840=VERTEX_POINT('',#10235);
#2841=VERTEX_POINT('',#10237);
#2842=VERTEX_POINT('',#10241);
#2843=VERTEX_POINT('',#10243);
#2844=VERTEX_POINT('',#10247);
#2845=VERTEX_POINT('',#10249);
#2846=VERTEX_POINT('',#10258);
#2847=VERTEX_POINT('',#10261);
#2848=VERTEX_POINT('',#10264);
#2849=VERTEX_POINT('',#10268);
#2850=VERTEX_POINT('',#10272);
#2851=VERTEX_POINT('',#10276);
#2852=VERTEX_POINT('',#10279);
#2853=VERTEX_POINT('',#10307);
#2854=VERTEX_POINT('',#10309);
#2855=VERTEX_POINT('',#10313);
#2856=VERTEX_POINT('',#10315);
#2857=VERTEX_POINT('',#10319);
#2858=VERTEX_POINT('',#10321);
#2859=VERTEX_POINT('',#10325);
#2860=VERTEX_POINT('',#10327);
#2861=VERTEX_POINT('',#10331);
#2862=VERTEX_POINT('',#10332);
#2863=VERTEX_POINT('',#10334);
#2864=VERTEX_POINT('',#10336);
#2865=VERTEX_POINT('',#10340);
#2866=VERTEX_POINT('',#10341);
#2867=VERTEX_POINT('',#10343);
#2868=VERTEX_POINT('',#10345);
#2869=VERTEX_POINT('',#10349);
#2870=VERTEX_POINT('',#10350);
#2871=VERTEX_POINT('',#10352);
#2872=VERTEX_POINT('',#10354);
#2873=VERTEX_POINT('',#10358);
#2874=VERTEX_POINT('',#10359);
#2875=VERTEX_POINT('',#10361);
#2876=VERTEX_POINT('',#10363);
#2877=VERTEX_POINT('',#10367);
#2878=VERTEX_POINT('',#10369);
#2879=VERTEX_POINT('',#10373);
#2880=VERTEX_POINT('',#10375);
#2881=VERTEX_POINT('',#10379);
#2882=VERTEX_POINT('',#10381);
#2883=VERTEX_POINT('',#10385);
#2884=VERTEX_POINT('',#10387);
#2885=VERTEX_POINT('',#10389);
#2886=VERTEX_POINT('',#10391);
#2887=VERTEX_POINT('',#10393);
#2888=VERTEX_POINT('',#10395);
#2889=VERTEX_POINT('',#10397);
#2890=VERTEX_POINT('',#10400);
#2891=VERTEX_POINT('',#10402);
#2892=VERTEX_POINT('',#10404);
#2893=VERTEX_POINT('',#10406);
#2894=VERTEX_POINT('',#10408);
#2895=VERTEX_POINT('',#10410);
#2896=VERTEX_POINT('',#10412);
#2897=VERTEX_POINT('',#10414);
#2898=VERTEX_POINT('',#10417);
#2899=VERTEX_POINT('',#10419);
#2900=VERTEX_POINT('',#10421);
#2901=VERTEX_POINT('',#10423);
#2902=VERTEX_POINT('',#10425);
#2903=VERTEX_POINT('',#10427);
#2904=VERTEX_POINT('',#10429);
#2905=VERTEX_POINT('',#10432);
#2906=VERTEX_POINT('',#10434);
#2907=VERTEX_POINT('',#10436);
#2908=VERTEX_POINT('',#10438);
#2909=VERTEX_POINT('',#10440);
#2910=VERTEX_POINT('',#10442);
#2911=VERTEX_POINT('',#10444);
#2912=VERTEX_POINT('',#10448);
#2913=VERTEX_POINT('',#10452);
#2914=VERTEX_POINT('',#10456);
#2915=VERTEX_POINT('',#10460);
#2916=VERTEX_POINT('',#10464);
#2917=VERTEX_POINT('',#10466);
#2918=VERTEX_POINT('',#10472);
#2919=VERTEX_POINT('',#10476);
#2920=VERTEX_POINT('',#10478);
#2921=VERTEX_POINT('',#10480);
#2922=VERTEX_POINT('',#10482);
#2923=VERTEX_POINT('',#10484);
#2924=VERTEX_POINT('',#10486);
#2925=VERTEX_POINT('',#10490);
#2926=VERTEX_POINT('',#10492);
#2927=VERTEX_POINT('',#10494);
#2928=VERTEX_POINT('',#10496);
#2929=VERTEX_POINT('',#10498);
#2930=VERTEX_POINT('',#10500);
#2931=VERTEX_POINT('',#10504);
#2932=VERTEX_POINT('',#10505);
#2933=VERTEX_POINT('',#10513);
#2934=VERTEX_POINT('',#10515);
#2935=VERTEX_POINT('',#10517);
#2936=VERTEX_POINT('',#10520);
#2937=VERTEX_POINT('',#10522);
#2938=VERTEX_POINT('',#10524);
#2939=VERTEX_POINT('',#10526);
#2940=VERTEX_POINT('',#10528);
#2941=VERTEX_POINT('',#10530);
#2942=VERTEX_POINT('',#10532);
#2943=VERTEX_POINT('',#10534);
#2944=VERTEX_POINT('',#10536);
#2945=VERTEX_POINT('',#10547);
#2946=VERTEX_POINT('',#10549);
#2947=VERTEX_POINT('',#10555);
#2948=VERTEX_POINT('',#10559);
#2949=VERTEX_POINT('',#10561);
#2950=VERTEX_POINT('',#10563);
#2951=VERTEX_POINT('',#10565);
#2952=VERTEX_POINT('',#10581);
#2953=VERTEX_POINT('',#10583);
#2954=VERTEX_POINT('',#10589);
#2955=VERTEX_POINT('',#10593);
#2956=VERTEX_POINT('',#10595);
#2957=VERTEX_POINT('',#10597);
#2958=VERTEX_POINT('',#10599);
#2959=VERTEX_POINT('',#10626);
#2960=VERTEX_POINT('',#10629);
#2961=VERTEX_POINT('',#10635);
#2962=VERTEX_POINT('',#10637);
#2963=VERTEX_POINT('',#10641);
#2964=VERTEX_POINT('',#10643);
#2965=VERTEX_POINT('',#10650);
#2966=VERTEX_POINT('',#10651);
#2967=VERTEX_POINT('',#10653);
#2968=VERTEX_POINT('',#10657);
#2969=VERTEX_POINT('',#10693);
#2970=VERTEX_POINT('',#10708);
#2971=VERTEX_POINT('',#10727);
#2972=VERTEX_POINT('',#10728);
#2973=VERTEX_POINT('',#10732);
#2974=VERTEX_POINT('',#10733);
#2975=VERTEX_POINT('',#10744);
#2976=VERTEX_POINT('',#10773);
#2977=VERTEX_POINT('',#10775);
#2978=VERTEX_POINT('',#10784);
#2979=VERTEX_POINT('',#10786);
#2980=VERTEX_POINT('',#10814);
#2981=VERTEX_POINT('',#10817);
#2982=VERTEX_POINT('',#10821);
#2983=VERTEX_POINT('',#10824);
#2984=VERTEX_POINT('',#10831);
#2985=VERTEX_POINT('',#10834);
#2986=VERTEX_POINT('',#10835);
#2987=VERTEX_POINT('',#10837);
#2988=VERTEX_POINT('',#10839);
#2989=VERTEX_POINT('',#10843);
#2990=VERTEX_POINT('',#10845);
#2991=VERTEX_POINT('',#10849);
#2992=VERTEX_POINT('',#10851);
#2993=VERTEX_POINT('',#10855);
#2994=VERTEX_POINT('',#10857);
#2995=VERTEX_POINT('',#10861);
#2996=VERTEX_POINT('',#10863);
#2997=VERTEX_POINT('',#10871);
#2998=VERTEX_POINT('',#10874);
#2999=EDGE_CURVE('',#2505,#2505,#2171,.T.);
#3000=EDGE_CURVE('',#2505,#2506,#1423,.T.);
#3001=EDGE_CURVE('',#2506,#2506,#2172,.T.);
#3002=EDGE_CURVE('',#2507,#2507,#2173,.T.);
#3003=EDGE_CURVE('',#2507,#2508,#1424,.T.);
#3004=EDGE_CURVE('',#2508,#2508,#2174,.T.);
#3005=EDGE_CURVE('',#2509,#2509,#2175,.T.);
#3006=EDGE_CURVE('',#2509,#2510,#1425,.T.);
#3007=EDGE_CURVE('',#2510,#2510,#2176,.T.);
#3008=EDGE_CURVE('',#2511,#2511,#2177,.T.);
#3009=EDGE_CURVE('',#2511,#2512,#1426,.T.);
#3010=EDGE_CURVE('',#2512,#2512,#2178,.T.);
#3011=EDGE_CURVE('',#2513,#2514,#1427,.T.);
#3012=EDGE_CURVE('',#2514,#2515,#1428,.T.);
#3013=EDGE_CURVE('',#2516,#2515,#1429,.T.);
#3014=EDGE_CURVE('',#2513,#2516,#1430,.T.);
#3015=EDGE_CURVE('',#2517,#2513,#1431,.T.);
#3016=EDGE_CURVE('',#2518,#2516,#1432,.T.);
#3017=EDGE_CURVE('',#2517,#2518,#1433,.T.);
#3018=EDGE_CURVE('',#2519,#2517,#1434,.T.);
#3019=EDGE_CURVE('',#2520,#2518,#1435,.T.);
#3020=EDGE_CURVE('',#2519,#2520,#1436,.T.);
#3021=EDGE_CURVE('',#2514,#2519,#1437,.T.);
#3022=EDGE_CURVE('',#2515,#2520,#1438,.T.);
#3023=EDGE_CURVE('',#2521,#2522,#1439,.T.);
#3024=EDGE_CURVE('',#2522,#2523,#1440,.T.);
#3025=EDGE_CURVE('',#2524,#2523,#1441,.T.);
#3026=EDGE_CURVE('',#2521,#2524,#1442,.T.);
#3027=EDGE_CURVE('',#2525,#2521,#1443,.T.);
#3028=EDGE_CURVE('',#2526,#2524,#1444,.T.);
#3029=EDGE_CURVE('',#2525,#2526,#1445,.T.);
#3030=EDGE_CURVE('',#2527,#2525,#1446,.T.);
#3031=EDGE_CURVE('',#2528,#2526,#1447,.T.);
#3032=EDGE_CURVE('',#2527,#2528,#1448,.T.);
#3033=EDGE_CURVE('',#2522,#2527,#1449,.T.);
#3034=EDGE_CURVE('',#2523,#2528,#1450,.T.);
#3035=EDGE_CURVE('',#2529,#2530,#1451,.T.);
#3036=EDGE_CURVE('',#2530,#2531,#1452,.T.);
#3037=EDGE_CURVE('',#2532,#2531,#1453,.T.);
#3038=EDGE_CURVE('',#2529,#2532,#1454,.T.);
#3039=EDGE_CURVE('',#2533,#2529,#1455,.T.);
#3040=EDGE_CURVE('',#2534,#2532,#1456,.T.);
#3041=EDGE_CURVE('',#2533,#2534,#1457,.T.);
#3042=EDGE_CURVE('',#2535,#2533,#1458,.T.);
#3043=EDGE_CURVE('',#2536,#2534,#1459,.T.);
#3044=EDGE_CURVE('',#2535,#2536,#1460,.T.);
#3045=EDGE_CURVE('',#2530,#2535,#1461,.T.);
#3046=EDGE_CURVE('',#2531,#2536,#1462,.T.);
#3047=EDGE_CURVE('',#2537,#2537,#2179,.T.);
#3048=EDGE_CURVE('',#2537,#2538,#1463,.T.);
#3049=EDGE_CURVE('',#2538,#2538,#213,.T.);
#3050=EDGE_CURVE('',#2539,#2539,#2180,.T.);
#3051=EDGE_CURVE('',#2539,#2540,#1464,.T.);
#3052=EDGE_CURVE('',#2540,#2540,#2181,.T.);
#3053=EDGE_CURVE('',#2541,#2541,#2182,.T.);
#3054=EDGE_CURVE('',#2541,#2542,#1465,.T.);
#3055=EDGE_CURVE('',#2542,#2542,#2183,.T.);
#3056=EDGE_CURVE('',#2543,#2543,#2184,.T.);
#3057=EDGE_CURVE('',#2543,#2544,#1466,.T.);
#3058=EDGE_CURVE('',#2544,#2544,#2185,.T.);
#3059=EDGE_CURVE('',#2545,#2545,#2186,.T.);
#3060=EDGE_CURVE('',#2545,#2546,#1467,.T.);
#3061=EDGE_CURVE('',#2546,#2546,#2187,.T.);
#3062=EDGE_CURVE('',#2547,#2547,#2188,.T.);
#3063=EDGE_CURVE('',#2547,#2548,#1468,.T.);
#3064=EDGE_CURVE('',#2548,#2548,#2189,.T.);
#3065=EDGE_CURVE('',#2549,#2549,#2190,.T.);
#3066=EDGE_CURVE('',#2550,#2550,#2191,.T.);
#3067=EDGE_CURVE('',#2550,#2549,#1469,.T.);
#3068=EDGE_CURVE('',#2551,#2551,#2192,.T.);
#3069=EDGE_CURVE('',#2551,#2552,#1470,.T.);
#3070=EDGE_CURVE('',#2552,#2552,#214,.T.);
#3071=EDGE_CURVE('',#2553,#2553,#2193,.T.);
#3072=EDGE_CURVE('',#2553,#2554,#1471,.T.);
#3073=EDGE_CURVE('',#2554,#2554,#2194,.T.);
#3074=EDGE_CURVE('',#2555,#2555,#2195,.T.);
#3075=EDGE_CURVE('',#2555,#2556,#1472,.T.);
#3076=EDGE_CURVE('',#2556,#2556,#2196,.T.);
#3077=EDGE_CURVE('',#2557,#2557,#2197,.T.);
#3078=EDGE_CURVE('',#2557,#2558,#1473,.T.);
#3079=EDGE_CURVE('',#2558,#2558,#2198,.T.);
#3080=EDGE_CURVE('',#2559,#2559,#2199,.T.);
#3081=EDGE_CURVE('',#2559,#2560,#1474,.T.);
#3082=EDGE_CURVE('',#2560,#2560,#2200,.T.);
#3083=EDGE_CURVE('',#2561,#2561,#2201,.T.);
#3084=EDGE_CURVE('',#2561,#2562,#1475,.T.);
#3085=EDGE_CURVE('',#2562,#2562,#2202,.T.);
#3086=EDGE_CURVE('',#2563,#2563,#2203,.T.);
#3087=EDGE_CURVE('',#2564,#2564,#2204,.T.);
#3088=EDGE_CURVE('',#2564,#2563,#1476,.T.);
#3089=EDGE_CURVE('',#2565,#2566,#1477,.T.);
#3090=EDGE_CURVE('',#2567,#2566,#2205,.T.);
#3091=EDGE_CURVE('',#2568,#2567,#1478,.T.);
#3092=EDGE_CURVE('',#2565,#2568,#2206,.T.);
#3093=EDGE_CURVE('',#2565,#2566,#1479,.T.);
#3094=EDGE_CURVE('',#2568,#2565,#2207,.T.);
#3095=EDGE_CURVE('',#2568,#2567,#1480,.T.);
#3096=EDGE_CURVE('',#2566,#2567,#2208,.T.);
#3097=EDGE_CURVE('',#2569,#2569,#2209,.T.);
#3098=EDGE_CURVE('',#2570,#2571,#1481,.T.);
#3099=EDGE_CURVE('',#2572,#2571,#2210,.T.);
#3100=EDGE_CURVE('',#2573,#2572,#1482,.T.);
#3101=EDGE_CURVE('',#2570,#2573,#2211,.T.);
#3102=EDGE_CURVE('',#2570,#2571,#1483,.T.);
#3103=EDGE_CURVE('',#2573,#2570,#2212,.T.);
#3104=EDGE_CURVE('',#2573,#2572,#1484,.T.);
#3105=EDGE_CURVE('',#2571,#2572,#2213,.T.);
#3106=EDGE_CURVE('',#2574,#2574,#2214,.T.);
#3107=EDGE_CURVE('',#2575,#2576,#1485,.T.);
#3108=EDGE_CURVE('',#2577,#2576,#2215,.T.);
#3109=EDGE_CURVE('',#2578,#2577,#1486,.T.);
#3110=EDGE_CURVE('',#2575,#2578,#2216,.T.);
#3111=EDGE_CURVE('',#2575,#2576,#1487,.T.);
#3112=EDGE_CURVE('',#2578,#2575,#2217,.T.);
#3113=EDGE_CURVE('',#2578,#2577,#1488,.T.);
#3114=EDGE_CURVE('',#2576,#2577,#2218,.T.);
#3115=EDGE_CURVE('',#2579,#2579,#2219,.T.);
#3116=EDGE_CURVE('',#2580,#2581,#1489,.T.);
#3117=EDGE_CURVE('',#2582,#2581,#2220,.T.);
#3118=EDGE_CURVE('',#2583,#2582,#1490,.T.);
#3119=EDGE_CURVE('',#2580,#2583,#2221,.T.);
#3120=EDGE_CURVE('',#2580,#2581,#1491,.T.);
#3121=EDGE_CURVE('',#2583,#2580,#2222,.T.);
#3122=EDGE_CURVE('',#2583,#2582,#1492,.T.);
#3123=EDGE_CURVE('',#2581,#2582,#2223,.T.);
#3124=EDGE_CURVE('',#2584,#2584,#2224,.T.);
#3125=EDGE_CURVE('',#2582,#2585,#1493,.T.);
#3126=EDGE_CURVE('',#2585,#2581,#1494,.T.);
#3127=EDGE_CURVE('',#2577,#2586,#1495,.T.);
#3128=EDGE_CURVE('',#2586,#2576,#1496,.T.);
#3129=EDGE_CURVE('',#2571,#2587,#1497,.T.);
#3130=EDGE_CURVE('',#2587,#2572,#1498,.T.);
#3131=EDGE_CURVE('',#2566,#2582,#1499,.T.);
#3132=EDGE_CURVE('',#2581,#2571,#1500,.T.);
#3133=EDGE_CURVE('',#2572,#2577,#1501,.T.);
#3134=EDGE_CURVE('',#2576,#2567,#1502,.T.);
#3135=EDGE_CURVE('',#2567,#2588,#1503,.T.);
#3136=EDGE_CURVE('',#2588,#2566,#1504,.T.);
#3137=EDGE_CURVE('',#2589,#2589,#2225,.T.);
#3138=EDGE_CURVE('',#2589,#2569,#1505,.T.);
#3139=EDGE_CURVE('',#2590,#2590,#2226,.T.);
#3140=EDGE_CURVE('',#2590,#2574,#1506,.T.);
#3141=EDGE_CURVE('',#2591,#2591,#2227,.T.);
#3142=EDGE_CURVE('',#2591,#2579,#1507,.T.);
#3143=EDGE_CURVE('',#2592,#2592,#2228,.T.);
#3144=EDGE_CURVE('',#2592,#2584,#1508,.T.);
#3145=EDGE_CURVE('',#2593,#2594,#1509,.T.);
#3146=EDGE_CURVE('',#2594,#2587,#1510,.T.);
#3147=EDGE_CURVE('',#2593,#2585,#1511,.T.);
#3148=EDGE_CURVE('',#2595,#2593,#1512,.T.);
#3149=EDGE_CURVE('',#2595,#2588,#1513,.T.);
#3150=EDGE_CURVE('',#2596,#2595,#1514,.T.);
#3151=EDGE_CURVE('',#2596,#2586,#1515,.T.);
#3152=EDGE_CURVE('',#2594,#2596,#1516,.T.);
#3153=EDGE_CURVE('',#2597,#2598,#1517,.T.);
#3154=EDGE_CURVE('',#2599,#2597,#2229,.T.);
#3155=EDGE_CURVE('',#2600,#2599,#1518,.T.);
#3156=EDGE_CURVE('',#2598,#2600,#2230,.T.);
#3157=EDGE_CURVE('',#2599,#2601,#2231,.T.);
#3158=EDGE_CURVE('',#2601,#2597,#2232,.T.);
#3159=EDGE_CURVE('',#2602,#2602,#2233,.T.);
#3160=EDGE_CURVE('',#2603,#2604,#2234,.T.);
#3161=EDGE_CURVE('',#2603,#2604,#2235,.T.);
#3162=EDGE_CURVE('',#2605,#2605,#2236,.T.);
#3163=EDGE_CURVE('',#2606,#2603,#1519,.T.);
#3164=EDGE_CURVE('',#2607,#2606,#2237,.T.);
#3165=EDGE_CURVE('',#2604,#2607,#1520,.T.);
#3166=EDGE_CURVE('',#2608,#2609,#2238,.T.);
#3167=EDGE_CURVE('',#2608,#2609,#2239,.T.);
#3168=EDGE_CURVE('',#2610,#2610,#2240,.T.);
#3169=EDGE_CURVE('',#2611,#2608,#1521,.T.);
#3170=EDGE_CURVE('',#2612,#2611,#2241,.T.);
#3171=EDGE_CURVE('',#2609,#2612,#1522,.T.);
#3172=EDGE_CURVE('',#2613,#2614,#2242,.T.);
#3173=EDGE_CURVE('',#2613,#2614,#2243,.T.);
#3174=EDGE_CURVE('',#2615,#2615,#2244,.T.);
#3175=EDGE_CURVE('',#2616,#2613,#1523,.T.);
#3176=EDGE_CURVE('',#2617,#2616,#2245,.T.);
#3177=EDGE_CURVE('',#2614,#2617,#1524,.T.);
#3178=EDGE_CURVE('',#2600,#2617,#2246,.T.);
#3179=EDGE_CURVE('',#2616,#2612,#2247,.T.);
#3180=EDGE_CURVE('',#2611,#2607,#2248,.T.);
#3181=EDGE_CURVE('',#2606,#2598,#2249,.T.);
#3182=EDGE_CURVE('',#2618,#2618,#2250,.T.);
#3183=EDGE_CURVE('',#2619,#2619,#2251,.T.);
#3184=EDGE_CURVE('',#2619,#2602,#1525,.T.);
#3185=EDGE_CURVE('',#2620,#2620,#2252,.T.);
#3186=EDGE_CURVE('',#2620,#2605,#1526,.T.);
#3187=EDGE_CURVE('',#2621,#2621,#2253,.T.);
#3188=EDGE_CURVE('',#2621,#2610,#1527,.T.);
#3189=EDGE_CURVE('',#2622,#2622,#2254,.T.);
#3190=EDGE_CURVE('',#2622,#2615,#1528,.T.);
#3191=EDGE_CURVE('',#2623,#2623,#2255,.T.);
#3192=EDGE_CURVE('',#2623,#2624,#1529,.T.);
#3193=EDGE_CURVE('',#2624,#2624,#2256,.T.);
#3194=EDGE_CURVE('',#2625,#2625,#2257,.T.);
#3195=EDGE_CURVE('',#2618,#2625,#1530,.T.);
#3196=EDGE_CURVE('',#2601,#2626,#1531,.T.);
#3197=EDGE_CURVE('',#2626,#2626,#2258,.T.);
#3198=EDGE_CURVE('',#2627,#2628,#1532,.T.);
#3199=EDGE_CURVE('',#2629,#2627,#2259,.T.);
#3200=EDGE_CURVE('',#2630,#2629,#1533,.T.);
#3201=EDGE_CURVE('',#2628,#2630,#2260,.T.);
#3202=EDGE_CURVE('',#2629,#2631,#2261,.T.);
#3203=EDGE_CURVE('',#2631,#2627,#2262,.T.);
#3204=EDGE_CURVE('',#2632,#2632,#2263,.T.);
#3205=EDGE_CURVE('',#2633,#2634,#2264,.T.);
#3206=EDGE_CURVE('',#2633,#2634,#2265,.T.);
#3207=EDGE_CURVE('',#2635,#2635,#2266,.T.);
#3208=EDGE_CURVE('',#2636,#2633,#1534,.T.);
#3209=EDGE_CURVE('',#2637,#2636,#2267,.T.);
#3210=EDGE_CURVE('',#2634,#2637,#1535,.T.);
#3211=EDGE_CURVE('',#2638,#2639,#2268,.T.);
#3212=EDGE_CURVE('',#2638,#2639,#2269,.T.);
#3213=EDGE_CURVE('',#2640,#2640,#2270,.T.);
#3214=EDGE_CURVE('',#2641,#2638,#1536,.T.);
#3215=EDGE_CURVE('',#2642,#2641,#2271,.T.);
#3216=EDGE_CURVE('',#2639,#2642,#1537,.T.);
#3217=EDGE_CURVE('',#2643,#2644,#2272,.T.);
#3218=EDGE_CURVE('',#2643,#2644,#2273,.T.);
#3219=EDGE_CURVE('',#2645,#2645,#2274,.T.);
#3220=EDGE_CURVE('',#2646,#2643,#1538,.T.);
#3221=EDGE_CURVE('',#2647,#2646,#2275,.T.);
#3222=EDGE_CURVE('',#2644,#2647,#1539,.T.);
#3223=EDGE_CURVE('',#2630,#2647,#2276,.T.);
#3224=EDGE_CURVE('',#2646,#2642,#2277,.T.);
#3225=EDGE_CURVE('',#2641,#2637,#2278,.T.);
#3226=EDGE_CURVE('',#2636,#2628,#2279,.T.);
#3227=EDGE_CURVE('',#2648,#2648,#2280,.T.);
#3228=EDGE_CURVE('',#2649,#2649,#2281,.T.);
#3229=EDGE_CURVE('',#2649,#2632,#1540,.T.);
#3230=EDGE_CURVE('',#2650,#2650,#2282,.T.);
#3231=EDGE_CURVE('',#2650,#2635,#1541,.T.);
#3232=EDGE_CURVE('',#2651,#2651,#2283,.T.);
#3233=EDGE_CURVE('',#2651,#2640,#1542,.T.);
#3234=EDGE_CURVE('',#2652,#2652,#2284,.T.);
#3235=EDGE_CURVE('',#2652,#2645,#1543,.T.);
#3236=EDGE_CURVE('',#2653,#2653,#2285,.T.);
#3237=EDGE_CURVE('',#2653,#2654,#1544,.T.);
#3238=EDGE_CURVE('',#2654,#2654,#2286,.T.);
#3239=EDGE_CURVE('',#2655,#2655,#2287,.T.);
#3240=EDGE_CURVE('',#2648,#2655,#1545,.T.);
#3241=EDGE_CURVE('',#2631,#2656,#1546,.T.);
#3242=EDGE_CURVE('',#2656,#2656,#2288,.T.);
#3243=EDGE_CURVE('',#2657,#2657,#2289,.T.);
#3244=EDGE_CURVE('',#2658,#2658,#2290,.T.);
#3245=EDGE_CURVE('',#2658,#2657,#1547,.T.);
#3246=EDGE_CURVE('',#2659,#2659,#2291,.T.);
#3247=EDGE_CURVE('',#2659,#2658,#1548,.T.);
#3248=EDGE_CURVE('',#2660,#2660,#2292,.T.);
#3249=EDGE_CURVE('',#2660,#2659,#1549,.T.);
#3250=EDGE_CURVE('',#2661,#2661,#2293,.T.);
#3251=EDGE_CURVE('',#2662,#2662,#2294,.F.);
#3252=EDGE_CURVE('',#2662,#2661,#1550,.T.);
#3253=EDGE_CURVE('',#2663,#2663,#2295,.F.);
#3254=EDGE_CURVE('',#2663,#2662,#1551,.T.);
#3255=EDGE_CURVE('',#2664,#2664,#2296,.T.);
#3256=EDGE_CURVE('',#2664,#2663,#1552,.T.);
#3257=EDGE_CURVE('',#2665,#2666,#1553,.T.);
#3258=EDGE_CURVE('',#2666,#2667,#1554,.T.);
#3259=EDGE_CURVE('',#2667,#2668,#1555,.T.);
#3260=EDGE_CURVE('',#2665,#2668,#1556,.T.);
#3261=EDGE_CURVE('',#2666,#2669,#1557,.T.);
#3262=EDGE_CURVE('',#2669,#2670,#1558,.T.);
#3263=EDGE_CURVE('',#2670,#2667,#1559,.T.);
#3264=EDGE_CURVE('',#2669,#2671,#1560,.T.);
#3265=EDGE_CURVE('',#2671,#2672,#1561,.T.);
#3266=EDGE_CURVE('',#2672,#2670,#1562,.T.);
#3267=EDGE_CURVE('',#2671,#2673,#1563,.T.);
#3268=EDGE_CURVE('',#2673,#2674,#1564,.T.);
#3269=EDGE_CURVE('',#2674,#2672,#1565,.T.);
#3270=EDGE_CURVE('',#2673,#2675,#1566,.T.);
#3271=EDGE_CURVE('',#2675,#2676,#1567,.T.);
#3272=EDGE_CURVE('',#2676,#2674,#1568,.T.);
#3273=EDGE_CURVE('',#2675,#2665,#1569,.T.);
#3274=EDGE_CURVE('',#2668,#2676,#1570,.T.);
#3275=EDGE_CURVE('',#2677,#2678,#2297,.T.);
#3276=EDGE_CURVE('',#2678,#2677,#2298,.T.);
#3277=EDGE_CURVE('',#2678,#2679,#2299,.T.);
#3278=EDGE_CURVE('',#2680,#2679,#2300,.T.);
#3279=EDGE_CURVE('',#2679,#2680,#2301,.T.);
#3280=EDGE_CURVE('',#2680,#2681,#1571,.T.);
#3281=EDGE_CURVE('',#2681,#2681,#2302,.T.);
#3282=EDGE_CURVE('',#2682,#2682,#2303,.T.);
#3283=EDGE_CURVE('',#2682,#2683,#1572,.T.);
#3284=EDGE_CURVE('',#2683,#2683,#2304,.T.);
#3285=EDGE_CURVE('',#2683,#2684,#1573,.T.);
#3286=EDGE_CURVE('',#2684,#2684,#2305,.T.);
#3287=EDGE_CURVE('',#2685,#2685,#2306,.T.);
#3288=EDGE_CURVE('',#2685,#2677,#1574,.T.);
#3289=EDGE_CURVE('',#2686,#2686,#2307,.T.);
#3290=EDGE_CURVE('',#2686,#2682,#1575,.T.);
#3291=EDGE_CURVE('',#2687,#2688,#2308,.T.);
#3292=EDGE_CURVE('',#2688,#2687,#2309,.T.);
#3293=EDGE_CURVE('',#2688,#2689,#2310,.T.);
#3294=EDGE_CURVE('',#2690,#2689,#2311,.T.);
#3295=EDGE_CURVE('',#2689,#2690,#2312,.T.);
#3296=EDGE_CURVE('',#2691,#2691,#2313,.T.);
#3297=EDGE_CURVE('',#2691,#2690,#1576,.T.);
#3298=EDGE_CURVE('',#2692,#2692,#2314,.T.);
#3299=EDGE_CURVE('',#2693,#2693,#2315,.T.);
#3300=EDGE_CURVE('',#2694,#2694,#2316,.T.);
#3301=EDGE_CURVE('',#2694,#2692,#1577,.T.);
#3302=EDGE_CURVE('',#2695,#2695,#2317,.T.);
#3303=EDGE_CURVE('',#2695,#2694,#1578,.T.);
#3304=EDGE_CURVE('',#2696,#2696,#2318,.T.);
#3305=EDGE_CURVE('',#2696,#2695,#1579,.T.);
#3306=EDGE_CURVE('',#2687,#2693,#1580,.T.);
#3307=EDGE_CURVE('',#2697,#2698,#2319,.T.);
#3308=EDGE_CURVE('',#2699,#2700,#2320,.T.);
#3309=EDGE_CURVE('',#2701,#2702,#2321,.T.);
#3310=EDGE_CURVE('',#2703,#2704,#2322,.T.);
#3311=EDGE_CURVE('',#2705,#2706,#2323,.T.);
#3312=EDGE_CURVE('',#2707,#2708,#2324,.T.);
#3313=EDGE_CURVE('',#2709,#2710,#2325,.T.);
#3314=EDGE_CURVE('',#2711,#2712,#2326,.T.);
#3315=EDGE_CURVE('',#2713,#2714,#215,.T.);
#3316=EDGE_CURVE('',#2715,#2713,#2327,.T.);
#3317=EDGE_CURVE('',#2716,#2715,#216,.T.);
#3318=EDGE_CURVE('',#2714,#2716,#2328,.T.);
#3319=EDGE_CURVE('',#2717,#2715,#2329,.T.);
#3320=EDGE_CURVE('',#2717,#2718,#217,.T.);
#3321=EDGE_CURVE('',#2719,#2718,#2330,.T.);
#3322=EDGE_CURVE('',#2719,#2720,#218,.T.);
#3323=EDGE_CURVE('',#2721,#2720,#2331,.T.);
#3324=EDGE_CURVE('',#2721,#2722,#219,.T.);
#3325=EDGE_CURVE('',#2722,#2723,#1581,.T.);
#3326=EDGE_CURVE('',#2723,#2723,#2332,.T.);
#3327=EDGE_CURVE('',#2722,#2724,#220,.T.);
#3328=EDGE_CURVE('',#2725,#2724,#2333,.T.);
#3329=EDGE_CURVE('',#2725,#2726,#221,.T.);
#3330=EDGE_CURVE('',#2727,#2726,#2334,.T.);
#3331=EDGE_CURVE('',#2727,#2728,#222,.T.);
#3332=EDGE_CURVE('',#2729,#2728,#2335,.T.);
#3333=EDGE_CURVE('',#2729,#2730,#223,.T.);
#3334=EDGE_CURVE('',#2731,#2730,#2336,.T.);
#3335=EDGE_CURVE('',#2731,#2732,#224,.T.);
#3336=EDGE_CURVE('',#2716,#2732,#2337,.T.);
#3337=EDGE_CURVE('',#2713,#2733,#2338,.T.);
#3338=EDGE_CURVE('',#2733,#2717,#2339,.T.);
#3339=EDGE_CURVE('',#2734,#2733,#225,.T.);
#3340=EDGE_CURVE('',#2718,#2734,#2340,.T.);
#3341=EDGE_CURVE('',#2734,#2735,#2341,.T.);
#3342=EDGE_CURVE('',#2735,#2719,#2342,.T.);
#3343=EDGE_CURVE('',#2736,#2735,#226,.T.);
#3344=EDGE_CURVE('',#2720,#2736,#2343,.T.);
#3345=EDGE_CURVE('',#2736,#2737,#2344,.T.);
#3346=EDGE_CURVE('',#2737,#2721,#2345,.T.);
#3347=EDGE_CURVE('',#2738,#2739,#227,.T.);
#3348=EDGE_CURVE('',#2724,#2738,#2346,.T.);
#3349=EDGE_CURVE('',#2739,#2737,#228,.T.);
#3350=EDGE_CURVE('',#2738,#2740,#2347,.T.);
#3351=EDGE_CURVE('',#2740,#2725,#2348,.T.);
#3352=EDGE_CURVE('',#2741,#2740,#229,.T.);
#3353=EDGE_CURVE('',#2726,#2741,#2349,.T.);
#3354=EDGE_CURVE('',#2741,#2742,#2350,.T.);
#3355=EDGE_CURVE('',#2742,#2727,#2351,.T.);
#3356=EDGE_CURVE('',#2743,#2742,#230,.T.);
#3357=EDGE_CURVE('',#2728,#2743,#2352,.T.);
#3358=EDGE_CURVE('',#2743,#2744,#2353,.T.);
#3359=EDGE_CURVE('',#2744,#2729,#2354,.T.);
#3360=EDGE_CURVE('',#2745,#2744,#231,.T.);
#3361=EDGE_CURVE('',#2730,#2745,#2355,.T.);
#3362=EDGE_CURVE('',#2746,#2746,#2356,.T.);
#3363=EDGE_CURVE('',#2746,#2739,#1582,.T.);
#3364=EDGE_CURVE('',#2747,#2714,#2357,.T.);
#3365=EDGE_CURVE('',#2747,#2748,#232,.T.);
#3366=EDGE_CURVE('',#2745,#2748,#2358,.T.);
#3367=EDGE_CURVE('',#2732,#2747,#2359,.T.);
#3368=EDGE_CURVE('',#2748,#2731,#2360,.T.);
#3369=EDGE_CURVE('',#2749,#2749,#2361,.T.);
#3370=EDGE_CURVE('',#2750,#2750,#2362,.T.);
#3371=EDGE_CURVE('',#2751,#2751,#2363,.T.);
#3372=EDGE_CURVE('',#2751,#2749,#1583,.T.);
#3373=EDGE_CURVE('',#2752,#2752,#2364,.T.);
#3374=EDGE_CURVE('',#2752,#2750,#1584,.T.);
#3375=EDGE_CURVE('',#2753,#2753,#2365,.T.);
#3376=EDGE_CURVE('',#2754,#2754,#2366,.T.);
#3377=EDGE_CURVE('',#2755,#2755,#2367,.T.);
#3378=EDGE_CURVE('',#2755,#2753,#1585,.T.);
#3379=EDGE_CURVE('',#2756,#2756,#2368,.T.);
#3380=EDGE_CURVE('',#2756,#2754,#1586,.T.);
#3381=EDGE_CURVE('',#2757,#2757,#2369,.T.);
#3382=EDGE_CURVE('',#2757,#2758,#1587,.T.);
#3383=EDGE_CURVE('',#2758,#2758,#2370,.T.);
#3384=EDGE_CURVE('',#2759,#2759,#2371,.T.);
#3385=EDGE_CURVE('',#2759,#2760,#1588,.T.);
#3386=EDGE_CURVE('',#2760,#2760,#2372,.T.);
#3387=EDGE_CURVE('',#2761,#2762,#1589,.T.);
#3388=EDGE_CURVE('',#2763,#2762,#2373,.T.);
#3389=EDGE_CURVE('',#2764,#2763,#1590,.T.);
#3390=EDGE_CURVE('',#2764,#2761,#2374,.T.);
#3391=EDGE_CURVE('',#2765,#2764,#1591,.T.);
#3392=EDGE_CURVE('',#2766,#2765,#2375,.T.);
#3393=EDGE_CURVE('',#2767,#2766,#1592,.T.);
#3394=EDGE_CURVE('',#2768,#2767,#1593,.T.);
#3395=EDGE_CURVE('',#2769,#2768,#1594,.T.);
#3396=EDGE_CURVE('',#2770,#2769,#2376,.T.);
#3397=EDGE_CURVE('',#2761,#2770,#1595,.T.);
#3398=EDGE_CURVE('',#2771,#2771,#2377,.T.);
#3399=EDGE_CURVE('',#2772,#2770,#1596,.T.);
#3400=EDGE_CURVE('',#2762,#2772,#1597,.T.);
#3401=EDGE_CURVE('',#2765,#2773,#1598,.T.);
#3402=EDGE_CURVE('',#2773,#2763,#1599,.T.);
#3403=EDGE_CURVE('',#2774,#2766,#1600,.T.);
#3404=EDGE_CURVE('',#2775,#2774,#1601,.T.);
#3405=EDGE_CURVE('',#2767,#2775,#1602,.T.);
#3406=EDGE_CURVE('',#2769,#2776,#1603,.T.);
#3407=EDGE_CURVE('',#2768,#2777,#1604,.T.);
#3408=EDGE_CURVE('',#2776,#2777,#1605,.T.);
#3409=EDGE_CURVE('',#2777,#2775,#1606,.T.);
#3410=EDGE_CURVE('',#2772,#2776,#2378,.T.);
#3411=EDGE_CURVE('',#2774,#2773,#2379,.T.);
#3412=EDGE_CURVE('',#2778,#2778,#2380,.T.);
#3413=EDGE_CURVE('',#2779,#2779,#2381,.T.);
#3414=EDGE_CURVE('',#2780,#2780,#2382,.T.);
#3415=EDGE_CURVE('',#2771,#2779,#1607,.T.);
#3416=EDGE_CURVE('',#2780,#2781,#1608,.T.);
#3417=EDGE_CURVE('',#2781,#2781,#2383,.T.);
#3418=EDGE_CURVE('',#2782,#2782,#2384,.T.);
#3419=EDGE_CURVE('',#2782,#2778,#1609,.T.);
#3420=EDGE_CURVE('',#2783,#2783,#2385,.T.);
#3421=EDGE_CURVE('',#2783,#2784,#1610,.T.);
#3422=EDGE_CURVE('',#2784,#2784,#2386,.T.);
#3423=EDGE_CURVE('',#2785,#2785,#2387,.T.);
#3424=EDGE_CURVE('',#2785,#2786,#1611,.T.);
#3425=EDGE_CURVE('',#2786,#2786,#2388,.T.);
#3426=EDGE_CURVE('',#2787,#2788,#1612,.T.);
#3427=EDGE_CURVE('',#2789,#2787,#2389,.T.);
#3428=EDGE_CURVE('',#2788,#2789,#2390,.T.);
#3429=EDGE_CURVE('',#2790,#2790,#233,.T.);
#3430=EDGE_CURVE('',#2790,#2789,#1613,.T.);
#3431=EDGE_CURVE('',#2791,#2787,#234,.T.);
#3432=EDGE_CURVE('',#2791,#2792,#2391,.T.);
#3433=EDGE_CURVE('',#2788,#2792,#235,.T.);
#3434=EDGE_CURVE('',#2792,#2791,#1614,.T.);
#3435=EDGE_CURVE('',#2793,#2794,#1615,.T.);
#3436=EDGE_CURVE('',#2794,#2793,#2392,.T.);
#3437=EDGE_CURVE('',#2795,#2796,#236,.T.);
#3438=EDGE_CURVE('',#2797,#2795,#237,.T.);
#3439=EDGE_CURVE('',#2796,#2797,#238,.T.);
#3440=EDGE_CURVE('',#2796,#2798,#1616,.T.);
#3441=EDGE_CURVE('',#2799,#2798,#239,.T.);
#3442=EDGE_CURVE('',#2799,#2800,#2393,.T.);
#3443=EDGE_CURVE('',#2801,#2800,#240,.T.);
#3444=EDGE_CURVE('',#2794,#2801,#241,.T.);
#3445=EDGE_CURVE('',#2798,#2793,#242,.T.);
#3446=EDGE_CURVE('',#2800,#2799,#1617,.T.);
#3447=EDGE_CURVE('',#2802,#2802,#2394,.T.);
#3448=EDGE_CURVE('',#2802,#2798,#1618,.T.);
#3449=EDGE_CURVE('',#2801,#2803,#1619,.T.);
#3450=EDGE_CURVE('',#2803,#2803,#2395,.T.);
#3451=EDGE_CURVE('',#2804,#2804,#2396,.T.);
#3452=EDGE_CURVE('',#2804,#2796,#1620,.T.);
#3453=EDGE_CURVE('',#2797,#2805,#1621,.T.);
#3454=EDGE_CURVE('',#2805,#2805,#2397,.T.);
#3455=EDGE_CURVE('',#2806,#2806,#2398,.T.);
#3456=EDGE_CURVE('',#2807,#2807,#2399,.T.);
#3457=EDGE_CURVE('',#2808,#2808,#2400,.T.);
#3458=EDGE_CURVE('',#2809,#2809,#2401,.T.);
#3459=EDGE_CURVE('',#2806,#2808,#1622,.T.);
#3460=EDGE_CURVE('',#2809,#2810,#1623,.T.);
#3461=EDGE_CURVE('',#2810,#2810,#2402,.T.);
#3462=EDGE_CURVE('',#2811,#2811,#2403,.T.);
#3463=EDGE_CURVE('',#2811,#2807,#1624,.T.);
#3464=EDGE_CURVE('',#2812,#2812,#2404,.T.);
#3465=EDGE_CURVE('',#2812,#2813,#1625,.T.);
#3466=EDGE_CURVE('',#2813,#2813,#2405,.T.);
#3467=EDGE_CURVE('',#2814,#2815,#1626,.T.);
#3468=EDGE_CURVE('',#2816,#2814,#2406,.T.);
#3469=EDGE_CURVE('',#2817,#2816,#1627,.T.);
#3470=EDGE_CURVE('',#2817,#2815,#2407,.T.);
#3471=EDGE_CURVE('',#2817,#2818,#1628,.T.);
#3472=EDGE_CURVE('',#2819,#2818,#2408,.T.);
#3473=EDGE_CURVE('',#2819,#2815,#1629,.T.);
#3474=EDGE_CURVE('',#2820,#2816,#1630,.T.);
#3475=EDGE_CURVE('',#2818,#2820,#1631,.T.);
#3476=EDGE_CURVE('',#2821,#2819,#1632,.T.);
#3477=EDGE_CURVE('',#2814,#2821,#1633,.T.);
#3478=EDGE_CURVE('',#2821,#2820,#2409,.T.);
#3479=EDGE_CURVE('',#2822,#2822,#2410,.T.);
#3480=EDGE_CURVE('',#2822,#2823,#1634,.T.);
#3481=EDGE_CURVE('',#2823,#2823,#2411,.T.);
#3482=EDGE_CURVE('',#2824,#2824,#2412,.T.);
#3483=EDGE_CURVE('',#2824,#2825,#1635,.T.);
#3484=EDGE_CURVE('',#2825,#2825,#2413,.T.);
#3485=EDGE_CURVE('',#2826,#2826,#2414,.T.);
#3486=EDGE_CURVE('',#2826,#2827,#1636,.T.);
#3487=EDGE_CURVE('',#2827,#2827,#2415,.T.);
#3488=EDGE_CURVE('',#2828,#2828,#2416,.T.);
#3489=EDGE_CURVE('',#2828,#2829,#1637,.T.);
#3490=EDGE_CURVE('',#2829,#2829,#2417,.T.);
#3491=EDGE_CURVE('',#2830,#2830,#2418,.T.);
#3492=EDGE_CURVE('',#2830,#2831,#1638,.T.);
#3493=EDGE_CURVE('',#2831,#2831,#2419,.T.);
#3494=EDGE_CURVE('',#2832,#2832,#2420,.T.);
#3495=EDGE_CURVE('',#2832,#2833,#1639,.T.);
#3496=EDGE_CURVE('',#2833,#2833,#2421,.T.);
#3497=EDGE_CURVE('',#2834,#2835,#1640,.T.);
#3498=EDGE_CURVE('',#2835,#2836,#1641,.T.);
#3499=EDGE_CURVE('',#2836,#2837,#1642,.T.);
#3500=EDGE_CURVE('',#2834,#2837,#1643,.T.);
#3501=EDGE_CURVE('',#2835,#2838,#1644,.T.);
#3502=EDGE_CURVE('',#2838,#2839,#1645,.T.);
#3503=EDGE_CURVE('',#2839,#2836,#1646,.T.);
#3504=EDGE_CURVE('',#2838,#2840,#1647,.T.);
#3505=EDGE_CURVE('',#2840,#2841,#1648,.T.);
#3506=EDGE_CURVE('',#2841,#2839,#1649,.T.);
#3507=EDGE_CURVE('',#2840,#2842,#1650,.T.);
#3508=EDGE_CURVE('',#2842,#2843,#1651,.T.);
#3509=EDGE_CURVE('',#2843,#2841,#1652,.T.);
#3510=EDGE_CURVE('',#2842,#2844,#1653,.T.);
#3511=EDGE_CURVE('',#2844,#2845,#1654,.T.);
#3512=EDGE_CURVE('',#2845,#2843,#1655,.T.);
#3513=EDGE_CURVE('',#2844,#2834,#1656,.T.);
#3514=EDGE_CURVE('',#2837,#2845,#1657,.T.);
#3515=EDGE_CURVE('',#2846,#2846,#2422,.T.);
#3516=EDGE_CURVE('',#2847,#2847,#2423,.T.);
#3517=EDGE_CURVE('',#2848,#2848,#2424,.T.);
#3518=EDGE_CURVE('',#2848,#2847,#1658,.T.);
#3519=EDGE_CURVE('',#2849,#2849,#2425,.T.);
#3520=EDGE_CURVE('',#2849,#2848,#1659,.T.);
#3521=EDGE_CURVE('',#2850,#2850,#2426,.T.);
#3522=EDGE_CURVE('',#2850,#2849,#1660,.T.);
#3523=EDGE_CURVE('',#2851,#2851,#2427,.T.);
#3524=EDGE_CURVE('',#2852,#2852,#2428,.F.);
#3525=EDGE_CURVE('',#2852,#2851,#1661,.T.);
#3526=EDGE_CURVE('',#2846,#2852,#1662,.T.);
#3527=EDGE_CURVE('',#2853,#2853,#2429,.T.);
#3528=EDGE_CURVE('',#2853,#2854,#1663,.T.);
#3529=EDGE_CURVE('',#2854,#2854,#2430,.T.);
#3530=EDGE_CURVE('',#2855,#2855,#2431,.T.);
#3531=EDGE_CURVE('',#2855,#2856,#1664,.T.);
#3532=EDGE_CURVE('',#2856,#2856,#2432,.T.);
#3533=EDGE_CURVE('',#2857,#2857,#2433,.T.);
#3534=EDGE_CURVE('',#2857,#2858,#1665,.T.);
#3535=EDGE_CURVE('',#2858,#2858,#2434,.T.);
#3536=EDGE_CURVE('',#2859,#2859,#2435,.T.);
#3537=EDGE_CURVE('',#2859,#2860,#1666,.T.);
#3538=EDGE_CURVE('',#2860,#2860,#2436,.T.);
#3539=EDGE_CURVE('',#2861,#2862,#2437,.T.);
#3540=EDGE_CURVE('',#2863,#2861,#1667,.T.);
#3541=EDGE_CURVE('',#2864,#2863,#2438,.T.);
#3542=EDGE_CURVE('',#2862,#2864,#1668,.T.);
#3543=EDGE_CURVE('',#2865,#2866,#2439,.T.);
#3544=EDGE_CURVE('',#2867,#2865,#1669,.T.);
#3545=EDGE_CURVE('',#2868,#2867,#2440,.T.);
#3546=EDGE_CURVE('',#2866,#2868,#1670,.T.);
#3547=EDGE_CURVE('',#2869,#2870,#2441,.T.);
#3548=EDGE_CURVE('',#2871,#2869,#1671,.T.);
#3549=EDGE_CURVE('',#2872,#2871,#2442,.T.);
#3550=EDGE_CURVE('',#2870,#2872,#1672,.T.);
#3551=EDGE_CURVE('',#2873,#2874,#1673,.T.);
#3552=EDGE_CURVE('',#2875,#2873,#2443,.T.);
#3553=EDGE_CURVE('',#2876,#2875,#1674,.T.);
#3554=EDGE_CURVE('',#2874,#2876,#2444,.T.);
#3555=EDGE_CURVE('',#2861,#2877,#2445,.T.);
#3556=EDGE_CURVE('',#2877,#2878,#1675,.T.);
#3557=EDGE_CURVE('',#2863,#2878,#2446,.T.);
#3558=EDGE_CURVE('',#2865,#2879,#2447,.T.);
#3559=EDGE_CURVE('',#2879,#2880,#1676,.T.);
#3560=EDGE_CURVE('',#2867,#2880,#2448,.T.);
#3561=EDGE_CURVE('',#2869,#2881,#2449,.T.);
#3562=EDGE_CURVE('',#2881,#2882,#1677,.T.);
#3563=EDGE_CURVE('',#2871,#2882,#2450,.T.);
#3564=EDGE_CURVE('',#2878,#2883,#1678,.T.);
#3565=EDGE_CURVE('',#2883,#2884,#1679,.T.);
#3566=EDGE_CURVE('',#2884,#2885,#1680,.T.);
#3567=EDGE_CURVE('',#2885,#2886,#2451,.T.);
#3568=EDGE_CURVE('',#2886,#2887,#1681,.T.);
#3569=EDGE_CURVE('',#2887,#2888,#1682,.T.);
#3570=EDGE_CURVE('',#2888,#2889,#1683,.T.);
#3571=EDGE_CURVE('',#2889,#2875,#2452,.T.);
#3572=EDGE_CURVE('',#2873,#2890,#2453,.T.);
#3573=EDGE_CURVE('',#2890,#2891,#1684,.T.);
#3574=EDGE_CURVE('',#2891,#2892,#1685,.T.);
#3575=EDGE_CURVE('',#2892,#2893,#1686,.T.);
#3576=EDGE_CURVE('',#2893,#2894,#2454,.T.);
#3577=EDGE_CURVE('',#2894,#2895,#1687,.T.);
#3578=EDGE_CURVE('',#2895,#2896,#1688,.T.);
#3579=EDGE_CURVE('',#2896,#2897,#1689,.T.);
#3580=EDGE_CURVE('',#2897,#2872,#2455,.T.);
#3581=EDGE_CURVE('',#2882,#2898,#1690,.T.);
#3582=EDGE_CURVE('',#2898,#2899,#1691,.T.);
#3583=EDGE_CURVE('',#2899,#2900,#1692,.T.);
#3584=EDGE_CURVE('',#2900,#2901,#2456,.T.);
#3585=EDGE_CURVE('',#2901,#2902,#1693,.T.);
#3586=EDGE_CURVE('',#2902,#2903,#1694,.T.);
#3587=EDGE_CURVE('',#2903,#2904,#1695,.T.);
#3588=EDGE_CURVE('',#2904,#2868,#2457,.T.);
#3589=EDGE_CURVE('',#2880,#2905,#1696,.T.);
#3590=EDGE_CURVE('',#2905,#2906,#1697,.T.);
#3591=EDGE_CURVE('',#2906,#2907,#1698,.T.);
#3592=EDGE_CURVE('',#2907,#2908,#2458,.T.);
#3593=EDGE_CURVE('',#2908,#2909,#1699,.T.);
#3594=EDGE_CURVE('',#2909,#2910,#1700,.T.);
#3595=EDGE_CURVE('',#2910,#2911,#1701,.T.);
#3596=EDGE_CURVE('',#2911,#2864,#2459,.T.);
#3597=EDGE_CURVE('',#2874,#2912,#2460,.T.);
#3598=EDGE_CURVE('',#2912,#2890,#1702,.T.);
#3599=EDGE_CURVE('',#2889,#2913,#1703,.T.);
#3600=EDGE_CURVE('',#2913,#2876,#2461,.T.);
#3601=EDGE_CURVE('',#2914,#2888,#1704,.T.);
#3602=EDGE_CURVE('',#2913,#2914,#1705,.T.);
#3603=EDGE_CURVE('',#2915,#2887,#1706,.T.);
#3604=EDGE_CURVE('',#2914,#2915,#1707,.T.);
#3605=EDGE_CURVE('',#2916,#2883,#1708,.T.);
#3606=EDGE_CURVE('',#2917,#2916,#1709,.T.);
#3607=EDGE_CURVE('',#2884,#2917,#1710,.T.);
#3608=EDGE_CURVE('',#2916,#2877,#1711,.T.);
#3609=EDGE_CURVE('',#2918,#2917,#1712,.T.);
#3610=EDGE_CURVE('',#2918,#2885,#1713,.T.);
#3611=EDGE_CURVE('',#2919,#2862,#2462,.T.);
#3612=EDGE_CURVE('',#2919,#2920,#1714,.T.);
#3613=EDGE_CURVE('',#2920,#2921,#1715,.T.);
#3614=EDGE_CURVE('',#2921,#2922,#1716,.T.);
#3615=EDGE_CURVE('',#2922,#2923,#2463,.T.);
#3616=EDGE_CURVE('',#2923,#2924,#2464,.T.);
#3617=EDGE_CURVE('',#2924,#2918,#2465,.T.);
#3618=EDGE_CURVE('',#2915,#2925,#1717,.T.);
#3619=EDGE_CURVE('',#2925,#2926,#2466,.T.);
#3620=EDGE_CURVE('',#2926,#2927,#2467,.T.);
#3621=EDGE_CURVE('',#2927,#2928,#2468,.T.);
#3622=EDGE_CURVE('',#2928,#2929,#1718,.T.);
#3623=EDGE_CURVE('',#2929,#2930,#1719,.T.);
#3624=EDGE_CURVE('',#2930,#2912,#1720,.T.);
#3625=EDGE_CURVE('',#2931,#2932,#2469,.T.);
#3626=EDGE_CURVE('',#2931,#2932,#2470,.T.);
#3627=EDGE_CURVE('',#2926,#2931,#1721,.T.);
#3628=EDGE_CURVE('',#2925,#2886,#1722,.T.);
#3629=EDGE_CURVE('',#2932,#2924,#1723,.T.);
#3630=EDGE_CURVE('',#2923,#2933,#1724,.T.);
#3631=EDGE_CURVE('',#2933,#2934,#2471,.T.);
#3632=EDGE_CURVE('',#2934,#2935,#1725,.T.);
#3633=EDGE_CURVE('',#2935,#2935,#2472,.T.);
#3634=EDGE_CURVE('',#2934,#2936,#2473,.T.);
#3635=EDGE_CURVE('',#2936,#2937,#1726,.T.);
#3636=EDGE_CURVE('',#2938,#2937,#2474,.T.);
#3637=EDGE_CURVE('',#2938,#2939,#1727,.T.);
#3638=EDGE_CURVE('',#2939,#2940,#2475,.T.);
#3639=EDGE_CURVE('',#2940,#2941,#1728,.T.);
#3640=EDGE_CURVE('',#2942,#2941,#2476,.T.);
#3641=EDGE_CURVE('',#2942,#2943,#1729,.T.);
#3642=EDGE_CURVE('',#2943,#2944,#2477,.T.);
#3643=EDGE_CURVE('',#2944,#2927,#1730,.T.);
#3644=EDGE_CURVE('',#2911,#2919,#1731,.T.);
#3645=EDGE_CURVE('',#2920,#2910,#1732,.T.);
#3646=EDGE_CURVE('',#2921,#2909,#1733,.T.);
#3647=EDGE_CURVE('',#2945,#2905,#1734,.T.);
#3648=EDGE_CURVE('',#2946,#2945,#1735,.T.);
#3649=EDGE_CURVE('',#2906,#2946,#1736,.T.);
#3650=EDGE_CURVE('',#2945,#2879,#1737,.T.);
#3651=EDGE_CURVE('',#2947,#2946,#1738,.T.);
#3652=EDGE_CURVE('',#2947,#2907,#1739,.T.);
#3653=EDGE_CURVE('',#2948,#2866,#2478,.T.);
#3654=EDGE_CURVE('',#2948,#2949,#1740,.T.);
#3655=EDGE_CURVE('',#2949,#2950,#1741,.T.);
#3656=EDGE_CURVE('',#2950,#2951,#1742,.T.);
#3657=EDGE_CURVE('',#2951,#2938,#2479,.T.);
#3658=EDGE_CURVE('',#2937,#2947,#2480,.T.);
#3659=EDGE_CURVE('',#2933,#2936,#2481,.T.);
#3660=EDGE_CURVE('',#2922,#2908,#1743,.T.);
#3661=EDGE_CURVE('',#2904,#2948,#1744,.T.);
#3662=EDGE_CURVE('',#2949,#2903,#1745,.T.);
#3663=EDGE_CURVE('',#2950,#2902,#1746,.T.);
#3664=EDGE_CURVE('',#2952,#2898,#1747,.T.);
#3665=EDGE_CURVE('',#2953,#2952,#1748,.T.);
#3666=EDGE_CURVE('',#2899,#2953,#1749,.T.);
#3667=EDGE_CURVE('',#2952,#2881,#1750,.T.);
#3668=EDGE_CURVE('',#2954,#2953,#1751,.T.);
#3669=EDGE_CURVE('',#2954,#2900,#1752,.T.);
#3670=EDGE_CURVE('',#2955,#2870,#2482,.T.);
#3671=EDGE_CURVE('',#2955,#2956,#1753,.T.);
#3672=EDGE_CURVE('',#2956,#2957,#1754,.T.);
#3673=EDGE_CURVE('',#2957,#2958,#1755,.T.);
#3674=EDGE_CURVE('',#2958,#2942,#2483,.T.);
#3675=EDGE_CURVE('',#2941,#2954,#2484,.T.);
#3676=EDGE_CURVE('',#2939,#2940,#2485,.T.);
#3677=EDGE_CURVE('',#2951,#2901,#1756,.T.);
#3678=EDGE_CURVE('',#2897,#2955,#1757,.T.);
#3679=EDGE_CURVE('',#2956,#2896,#1758,.T.);
#3680=EDGE_CURVE('',#2930,#2891,#1759,.T.);
#3681=EDGE_CURVE('',#2892,#2929,#1760,.T.);
#3682=EDGE_CURVE('',#2957,#2895,#1761,.T.);
#3683=EDGE_CURVE('',#2943,#2944,#2486,.T.);
#3684=EDGE_CURVE('',#2958,#2894,#1762,.T.);
#3685=EDGE_CURVE('',#2928,#2893,#1763,.T.);
#3686=EDGE_CURVE('',#2959,#2959,#2487,.T.);
#3687=EDGE_CURVE('',#2959,#2960,#1764,.T.);
#3688=EDGE_CURVE('',#2960,#2960,#2488,.T.);
#3689=EDGE_CURVE('',#2961,#2961,#2489,.T.);
#3690=EDGE_CURVE('',#2961,#2962,#1765,.T.);
#3691=EDGE_CURVE('',#2962,#2962,#2490,.T.);
#3692=EDGE_CURVE('',#2963,#2963,#2491,.T.);
#3693=EDGE_CURVE('',#2963,#2964,#1766,.T.);
#3694=EDGE_CURVE('',#2964,#2964,#2492,.T.);
#3695=EDGE_CURVE('',#2965,#2966,#1767,.T.);
#3696=EDGE_CURVE('',#2967,#2965,#2493,.T.);
#3697=EDGE_CURVE('',#2966,#2967,#2494,.T.);
#3698=EDGE_CURVE('',#2968,#2968,#243,.T.);
#3699=EDGE_CURVE('',#2968,#2967,#1768,.T.);
#3700=EDGE_CURVE('',#2969,#2965,#244,.T.);
#3701=EDGE_CURVE('',#2969,#2970,#2495,.T.);
#3702=EDGE_CURVE('',#2966,#2970,#245,.T.);
#3703=EDGE_CURVE('',#2970,#2969,#1769,.T.);
#3704=EDGE_CURVE('',#2971,#2972,#1770,.T.);
#3705=EDGE_CURVE('',#2972,#2971,#2496,.T.);
#3706=EDGE_CURVE('',#2973,#2974,#246,.T.);
#3707=EDGE_CURVE('',#2975,#2973,#247,.T.);
#3708=EDGE_CURVE('',#2974,#2975,#248,.T.);
#3709=EDGE_CURVE('',#2974,#2976,#1771,.T.);
#3710=EDGE_CURVE('',#2977,#2976,#249,.T.);
#3711=EDGE_CURVE('',#2977,#2978,#2497,.T.);
#3712=EDGE_CURVE('',#2979,#2978,#250,.T.);
#3713=EDGE_CURVE('',#2972,#2979,#251,.T.);
#3714=EDGE_CURVE('',#2976,#2971,#252,.T.);
#3715=EDGE_CURVE('',#2978,#2977,#1772,.T.);
#3716=EDGE_CURVE('',#2980,#2980,#2498,.T.);
#3717=EDGE_CURVE('',#2980,#2976,#1773,.T.);
#3718=EDGE_CURVE('',#2979,#2981,#1774,.T.);
#3719=EDGE_CURVE('',#2981,#2981,#2499,.T.);
#3720=EDGE_CURVE('',#2982,#2982,#2500,.T.);
#3721=EDGE_CURVE('',#2982,#2974,#1775,.T.);
#3722=EDGE_CURVE('',#2975,#2983,#1776,.T.);
#3723=EDGE_CURVE('',#2983,#2983,#2501,.T.);
#3724=EDGE_CURVE('',#2984,#2984,#2502,.T.);
#3725=EDGE_CURVE('',#2985,#2986,#1777,.T.);
#3726=EDGE_CURVE('',#2985,#2987,#1778,.T.);
#3727=EDGE_CURVE('',#2987,#2988,#1779,.T.);
#3728=EDGE_CURVE('',#2986,#2988,#1780,.T.);
#3729=EDGE_CURVE('',#2989,#2985,#1781,.T.);
#3730=EDGE_CURVE('',#2989,#2990,#1782,.T.);
#3731=EDGE_CURVE('',#2990,#2987,#1783,.T.);
#3732=EDGE_CURVE('',#2991,#2989,#1784,.T.);
#3733=EDGE_CURVE('',#2991,#2992,#1785,.T.);
#3734=EDGE_CURVE('',#2992,#2990,#1786,.T.);
#3735=EDGE_CURVE('',#2993,#2991,#1787,.T.);
#3736=EDGE_CURVE('',#2993,#2994,#1788,.T.);
#3737=EDGE_CURVE('',#2994,#2992,#1789,.T.);
#3738=EDGE_CURVE('',#2995,#2993,#1790,.T.);
#3739=EDGE_CURVE('',#2995,#2996,#1791,.T.);
#3740=EDGE_CURVE('',#2996,#2994,#1792,.T.);
#3741=EDGE_CURVE('',#2986,#2995,#1793,.T.);
#3742=EDGE_CURVE('',#2988,#2996,#1794,.T.);
#3743=EDGE_CURVE('',#2997,#2997,#2503,.T.);
#3744=EDGE_CURVE('',#2998,#2998,#2504,.T.);
#3745=EDGE_CURVE('',#2998,#2997,#1795,.T.);
#3746=EDGE_CURVE('',#2984,#2998,#1796,.T.);
#3747=ORIENTED_EDGE('',*,*,#2999,.F.);
#3748=ORIENTED_EDGE('',*,*,#3000,.T.);
#3749=ORIENTED_EDGE('',*,*,#3001,.F.);
#3750=ORIENTED_EDGE('',*,*,#3000,.F.);
#3751=ORIENTED_EDGE('',*,*,#3002,.F.);
#3752=ORIENTED_EDGE('',*,*,#3003,.T.);
#3753=ORIENTED_EDGE('',*,*,#3004,.F.);
#3754=ORIENTED_EDGE('',*,*,#3003,.F.);
#3755=ORIENTED_EDGE('',*,*,#3005,.F.);
#3756=ORIENTED_EDGE('',*,*,#3006,.T.);
#3757=ORIENTED_EDGE('',*,*,#3007,.F.);
#3758=ORIENTED_EDGE('',*,*,#3006,.F.);
#3759=ORIENTED_EDGE('',*,*,#3008,.F.);
#3760=ORIENTED_EDGE('',*,*,#3009,.T.);
#3761=ORIENTED_EDGE('',*,*,#3010,.F.);
#3762=ORIENTED_EDGE('',*,*,#3009,.F.);
#3763=ORIENTED_EDGE('',*,*,#3011,.T.);
#3764=ORIENTED_EDGE('',*,*,#3012,.T.);
#3765=ORIENTED_EDGE('',*,*,#3013,.F.);
#3766=ORIENTED_EDGE('',*,*,#3014,.F.);
#3767=ORIENTED_EDGE('',*,*,#3015,.T.);
#3768=ORIENTED_EDGE('',*,*,#3014,.T.);
#3769=ORIENTED_EDGE('',*,*,#3016,.F.);
#3770=ORIENTED_EDGE('',*,*,#3017,.F.);
#3771=ORIENTED_EDGE('',*,*,#3018,.T.);
#3772=ORIENTED_EDGE('',*,*,#3017,.T.);
#3773=ORIENTED_EDGE('',*,*,#3019,.F.);
#3774=ORIENTED_EDGE('',*,*,#3020,.F.);
#3775=ORIENTED_EDGE('',*,*,#3021,.T.);
#3776=ORIENTED_EDGE('',*,*,#3020,.T.);
#3777=ORIENTED_EDGE('',*,*,#3022,.F.);
#3778=ORIENTED_EDGE('',*,*,#3012,.F.);
#3779=ORIENTED_EDGE('',*,*,#3022,.T.);
#3780=ORIENTED_EDGE('',*,*,#3019,.T.);
#3781=ORIENTED_EDGE('',*,*,#3016,.T.);
#3782=ORIENTED_EDGE('',*,*,#3013,.T.);
#3783=ORIENTED_EDGE('',*,*,#3001,.T.);
#3784=ORIENTED_EDGE('',*,*,#3004,.T.);
#3785=ORIENTED_EDGE('',*,*,#3007,.T.);
#3786=ORIENTED_EDGE('',*,*,#3010,.T.);
#3787=ORIENTED_EDGE('',*,*,#3021,.F.);
#3788=ORIENTED_EDGE('',*,*,#3011,.F.);
#3789=ORIENTED_EDGE('',*,*,#3015,.F.);
#3790=ORIENTED_EDGE('',*,*,#3018,.F.);
#3791=ORIENTED_EDGE('',*,*,#2999,.T.);
#3792=ORIENTED_EDGE('',*,*,#3002,.T.);
#3793=ORIENTED_EDGE('',*,*,#3005,.T.);
#3794=ORIENTED_EDGE('',*,*,#3008,.T.);
#3795=ORIENTED_EDGE('',*,*,#3023,.T.);
#3796=ORIENTED_EDGE('',*,*,#3024,.T.);
#3797=ORIENTED_EDGE('',*,*,#3025,.F.);
#3798=ORIENTED_EDGE('',*,*,#3026,.F.);
#3799=ORIENTED_EDGE('',*,*,#3027,.T.);
#3800=ORIENTED_EDGE('',*,*,#3026,.T.);
#3801=ORIENTED_EDGE('',*,*,#3028,.F.);
#3802=ORIENTED_EDGE('',*,*,#3029,.F.);
#3803=ORIENTED_EDGE('',*,*,#3030,.T.);
#3804=ORIENTED_EDGE('',*,*,#3029,.T.);
#3805=ORIENTED_EDGE('',*,*,#3031,.F.);
#3806=ORIENTED_EDGE('',*,*,#3032,.F.);
#3807=ORIENTED_EDGE('',*,*,#3033,.T.);
#3808=ORIENTED_EDGE('',*,*,#3032,.T.);
#3809=ORIENTED_EDGE('',*,*,#3034,.F.);
#3810=ORIENTED_EDGE('',*,*,#3024,.F.);
#3811=ORIENTED_EDGE('',*,*,#3034,.T.);
#3812=ORIENTED_EDGE('',*,*,#3031,.T.);
#3813=ORIENTED_EDGE('',*,*,#3028,.T.);
#3814=ORIENTED_EDGE('',*,*,#3025,.T.);
#3815=ORIENTED_EDGE('',*,*,#3033,.F.);
#3816=ORIENTED_EDGE('',*,*,#3023,.F.);
#3817=ORIENTED_EDGE('',*,*,#3027,.F.);
#3818=ORIENTED_EDGE('',*,*,#3030,.F.);
#3819=ORIENTED_EDGE('',*,*,#3035,.T.);
#3820=ORIENTED_EDGE('',*,*,#3036,.T.);
#3821=ORIENTED_EDGE('',*,*,#3037,.F.);
#3822=ORIENTED_EDGE('',*,*,#3038,.F.);
#3823=ORIENTED_EDGE('',*,*,#3039,.T.);
#3824=ORIENTED_EDGE('',*,*,#3038,.T.);
#3825=ORIENTED_EDGE('',*,*,#3040,.F.);
#3826=ORIENTED_EDGE('',*,*,#3041,.F.);
#3827=ORIENTED_EDGE('',*,*,#3042,.T.);
#3828=ORIENTED_EDGE('',*,*,#3041,.T.);
#3829=ORIENTED_EDGE('',*,*,#3043,.F.);
#3830=ORIENTED_EDGE('',*,*,#3044,.F.);
#3831=ORIENTED_EDGE('',*,*,#3045,.T.);
#3832=ORIENTED_EDGE('',*,*,#3044,.T.);
#3833=ORIENTED_EDGE('',*,*,#3046,.F.);
#3834=ORIENTED_EDGE('',*,*,#3036,.F.);
#3835=ORIENTED_EDGE('',*,*,#3046,.T.);
#3836=ORIENTED_EDGE('',*,*,#3043,.T.);
#3837=ORIENTED_EDGE('',*,*,#3040,.T.);
#3838=ORIENTED_EDGE('',*,*,#3037,.T.);
#3839=ORIENTED_EDGE('',*,*,#3045,.F.);
#3840=ORIENTED_EDGE('',*,*,#3035,.F.);
#3841=ORIENTED_EDGE('',*,*,#3039,.F.);
#3842=ORIENTED_EDGE('',*,*,#3042,.F.);
#3843=ORIENTED_EDGE('',*,*,#3047,.F.);
#3844=ORIENTED_EDGE('',*,*,#3048,.T.);
#3845=ORIENTED_EDGE('',*,*,#3049,.F.);
#3846=ORIENTED_EDGE('',*,*,#3048,.F.);
#3847=ORIENTED_EDGE('',*,*,#3050,.F.);
#3848=ORIENTED_EDGE('',*,*,#3051,.T.);
#3849=ORIENTED_EDGE('',*,*,#3052,.F.);
#3850=ORIENTED_EDGE('',*,*,#3051,.F.);
#3851=ORIENTED_EDGE('',*,*,#3050,.T.);
#3852=ORIENTED_EDGE('',*,*,#3053,.F.);
#3853=ORIENTED_EDGE('',*,*,#3054,.T.);
#3854=ORIENTED_EDGE('',*,*,#3055,.F.);
#3855=ORIENTED_EDGE('',*,*,#3054,.F.);
#3856=ORIENTED_EDGE('',*,*,#3053,.T.);
#3857=ORIENTED_EDGE('',*,*,#3056,.F.);
#3858=ORIENTED_EDGE('',*,*,#3057,.T.);
#3859=ORIENTED_EDGE('',*,*,#3058,.F.);
#3860=ORIENTED_EDGE('',*,*,#3057,.F.);
#3861=ORIENTED_EDGE('',*,*,#3056,.T.);
#3862=ORIENTED_EDGE('',*,*,#3059,.F.);
#3863=ORIENTED_EDGE('',*,*,#3060,.T.);
#3864=ORIENTED_EDGE('',*,*,#3061,.F.);
#3865=ORIENTED_EDGE('',*,*,#3060,.F.);
#3866=ORIENTED_EDGE('',*,*,#3059,.T.);
#3867=ORIENTED_EDGE('',*,*,#3062,.F.);
#3868=ORIENTED_EDGE('',*,*,#3063,.T.);
#3869=ORIENTED_EDGE('',*,*,#3064,.F.);
#3870=ORIENTED_EDGE('',*,*,#3063,.F.);
#3871=ORIENTED_EDGE('',*,*,#3062,.T.);
#3872=ORIENTED_EDGE('',*,*,#3065,.F.);
#3873=ORIENTED_EDGE('',*,*,#3066,.F.);
#3874=ORIENTED_EDGE('',*,*,#3067,.T.);
#3875=ORIENTED_EDGE('',*,*,#3065,.T.);
#3876=ORIENTED_EDGE('',*,*,#3067,.F.);
#3877=ORIENTED_EDGE('',*,*,#3049,.T.);
#3878=ORIENTED_EDGE('',*,*,#3068,.F.);
#3879=ORIENTED_EDGE('',*,*,#3069,.T.);
#3880=ORIENTED_EDGE('',*,*,#3070,.F.);
#3881=ORIENTED_EDGE('',*,*,#3069,.F.);
#3882=ORIENTED_EDGE('',*,*,#3071,.F.);
#3883=ORIENTED_EDGE('',*,*,#3072,.T.);
#3884=ORIENTED_EDGE('',*,*,#3073,.F.);
#3885=ORIENTED_EDGE('',*,*,#3072,.F.);
#3886=ORIENTED_EDGE('',*,*,#3071,.T.);
#3887=ORIENTED_EDGE('',*,*,#3074,.F.);
#3888=ORIENTED_EDGE('',*,*,#3075,.T.);
#3889=ORIENTED_EDGE('',*,*,#3076,.F.);
#3890=ORIENTED_EDGE('',*,*,#3075,.F.);
#3891=ORIENTED_EDGE('',*,*,#3074,.T.);
#3892=ORIENTED_EDGE('',*,*,#3077,.F.);
#3893=ORIENTED_EDGE('',*,*,#3078,.T.);
#3894=ORIENTED_EDGE('',*,*,#3079,.F.);
#3895=ORIENTED_EDGE('',*,*,#3078,.F.);
#3896=ORIENTED_EDGE('',*,*,#3077,.T.);
#3897=ORIENTED_EDGE('',*,*,#3080,.F.);
#3898=ORIENTED_EDGE('',*,*,#3081,.T.);
#3899=ORIENTED_EDGE('',*,*,#3082,.F.);
#3900=ORIENTED_EDGE('',*,*,#3081,.F.);
#3901=ORIENTED_EDGE('',*,*,#3080,.T.);
#3902=ORIENTED_EDGE('',*,*,#3083,.F.);
#3903=ORIENTED_EDGE('',*,*,#3084,.T.);
#3904=ORIENTED_EDGE('',*,*,#3085,.F.);
#3905=ORIENTED_EDGE('',*,*,#3084,.F.);
#3906=ORIENTED_EDGE('',*,*,#3083,.T.);
#3907=ORIENTED_EDGE('',*,*,#3086,.F.);
#3908=ORIENTED_EDGE('',*,*,#3087,.F.);
#3909=ORIENTED_EDGE('',*,*,#3088,.T.);
#3910=ORIENTED_EDGE('',*,*,#3086,.T.);
#3911=ORIENTED_EDGE('',*,*,#3088,.F.);
#3912=ORIENTED_EDGE('',*,*,#3070,.T.);
#3913=ORIENTED_EDGE('',*,*,#3089,.T.);
#3914=ORIENTED_EDGE('',*,*,#3090,.F.);
#3915=ORIENTED_EDGE('',*,*,#3091,.F.);
#3916=ORIENTED_EDGE('',*,*,#3092,.F.);
#3917=ORIENTED_EDGE('',*,*,#3093,.F.);
#3918=ORIENTED_EDGE('',*,*,#3094,.F.);
#3919=ORIENTED_EDGE('',*,*,#3095,.T.);
#3920=ORIENTED_EDGE('',*,*,#3096,.F.);
#3921=ORIENTED_EDGE('',*,*,#3092,.T.);
#3922=ORIENTED_EDGE('',*,*,#3094,.T.);
#3923=ORIENTED_EDGE('',*,*,#3097,.F.);
#3924=ORIENTED_EDGE('',*,*,#3098,.T.);
#3925=ORIENTED_EDGE('',*,*,#3099,.F.);
#3926=ORIENTED_EDGE('',*,*,#3100,.F.);
#3927=ORIENTED_EDGE('',*,*,#3101,.F.);
#3928=ORIENTED_EDGE('',*,*,#3102,.F.);
#3929=ORIENTED_EDGE('',*,*,#3103,.F.);
#3930=ORIENTED_EDGE('',*,*,#3104,.T.);
#3931=ORIENTED_EDGE('',*,*,#3105,.F.);
#3932=ORIENTED_EDGE('',*,*,#3103,.T.);
#3933=ORIENTED_EDGE('',*,*,#3101,.T.);
#3934=ORIENTED_EDGE('',*,*,#3106,.F.);
#3935=ORIENTED_EDGE('',*,*,#3107,.T.);
#3936=ORIENTED_EDGE('',*,*,#3108,.F.);
#3937=ORIENTED_EDGE('',*,*,#3109,.F.);
#3938=ORIENTED_EDGE('',*,*,#3110,.F.);
#3939=ORIENTED_EDGE('',*,*,#3111,.F.);
#3940=ORIENTED_EDGE('',*,*,#3112,.F.);
#3941=ORIENTED_EDGE('',*,*,#3113,.T.);
#3942=ORIENTED_EDGE('',*,*,#3114,.F.);
#3943=ORIENTED_EDGE('',*,*,#3112,.T.);
#3944=ORIENTED_EDGE('',*,*,#3110,.T.);
#3945=ORIENTED_EDGE('',*,*,#3115,.F.);
#3946=ORIENTED_EDGE('',*,*,#3116,.T.);
#3947=ORIENTED_EDGE('',*,*,#3117,.F.);
#3948=ORIENTED_EDGE('',*,*,#3118,.F.);
#3949=ORIENTED_EDGE('',*,*,#3119,.F.);
#3950=ORIENTED_EDGE('',*,*,#3120,.F.);
#3951=ORIENTED_EDGE('',*,*,#3121,.F.);
#3952=ORIENTED_EDGE('',*,*,#3122,.T.);
#3953=ORIENTED_EDGE('',*,*,#3123,.F.);
#3954=ORIENTED_EDGE('',*,*,#3119,.T.);
#3955=ORIENTED_EDGE('',*,*,#3121,.T.);
#3956=ORIENTED_EDGE('',*,*,#3124,.F.);
#3957=ORIENTED_EDGE('',*,*,#3123,.T.);
#3958=ORIENTED_EDGE('',*,*,#3125,.T.);
#3959=ORIENTED_EDGE('',*,*,#3126,.T.);
#3960=ORIENTED_EDGE('',*,*,#3114,.T.);
#3961=ORIENTED_EDGE('',*,*,#3127,.T.);
#3962=ORIENTED_EDGE('',*,*,#3128,.T.);
#3963=ORIENTED_EDGE('',*,*,#3099,.T.);
#3964=ORIENTED_EDGE('',*,*,#3129,.T.);
#3965=ORIENTED_EDGE('',*,*,#3130,.T.);
#3966=ORIENTED_EDGE('',*,*,#3090,.T.);
#3967=ORIENTED_EDGE('',*,*,#3131,.T.);
#3968=ORIENTED_EDGE('',*,*,#3117,.T.);
#3969=ORIENTED_EDGE('',*,*,#3132,.T.);
#3970=ORIENTED_EDGE('',*,*,#3105,.T.);
#3971=ORIENTED_EDGE('',*,*,#3133,.T.);
#3972=ORIENTED_EDGE('',*,*,#3108,.T.);
#3973=ORIENTED_EDGE('',*,*,#3134,.T.);
#3974=ORIENTED_EDGE('',*,*,#3073,.T.);
#3975=ORIENTED_EDGE('',*,*,#3076,.T.);
#3976=ORIENTED_EDGE('',*,*,#3079,.T.);
#3977=ORIENTED_EDGE('',*,*,#3082,.T.);
#3978=ORIENTED_EDGE('',*,*,#3085,.T.);
#3979=ORIENTED_EDGE('',*,*,#3064,.T.);
#3980=ORIENTED_EDGE('',*,*,#3061,.T.);
#3981=ORIENTED_EDGE('',*,*,#3058,.T.);
#3982=ORIENTED_EDGE('',*,*,#3055,.T.);
#3983=ORIENTED_EDGE('',*,*,#3052,.T.);
#3984=ORIENTED_EDGE('',*,*,#3096,.T.);
#3985=ORIENTED_EDGE('',*,*,#3135,.T.);
#3986=ORIENTED_EDGE('',*,*,#3136,.T.);
#3987=ORIENTED_EDGE('',*,*,#3137,.F.);
#3988=ORIENTED_EDGE('',*,*,#3138,.T.);
#3989=ORIENTED_EDGE('',*,*,#3097,.T.);
#3990=ORIENTED_EDGE('',*,*,#3138,.F.);
#3991=ORIENTED_EDGE('',*,*,#3139,.F.);
#3992=ORIENTED_EDGE('',*,*,#3140,.T.);
#3993=ORIENTED_EDGE('',*,*,#3106,.T.);
#3994=ORIENTED_EDGE('',*,*,#3140,.F.);
#3995=ORIENTED_EDGE('',*,*,#3141,.F.);
#3996=ORIENTED_EDGE('',*,*,#3142,.T.);
#3997=ORIENTED_EDGE('',*,*,#3115,.T.);
#3998=ORIENTED_EDGE('',*,*,#3142,.F.);
#3999=ORIENTED_EDGE('',*,*,#3143,.F.);
#4000=ORIENTED_EDGE('',*,*,#3144,.T.);
#4001=ORIENTED_EDGE('',*,*,#3124,.T.);
#4002=ORIENTED_EDGE('',*,*,#3144,.F.);
#4003=ORIENTED_EDGE('',*,*,#3145,.T.);
#4004=ORIENTED_EDGE('',*,*,#3146,.T.);
#4005=ORIENTED_EDGE('',*,*,#3129,.F.);
#4006=ORIENTED_EDGE('',*,*,#3098,.F.);
#4007=ORIENTED_EDGE('',*,*,#3102,.T.);
#4008=ORIENTED_EDGE('',*,*,#3132,.F.);
#4009=ORIENTED_EDGE('',*,*,#3116,.F.);
#4010=ORIENTED_EDGE('',*,*,#3120,.T.);
#4011=ORIENTED_EDGE('',*,*,#3126,.F.);
#4012=ORIENTED_EDGE('',*,*,#3147,.F.);
#4013=ORIENTED_EDGE('',*,*,#3148,.T.);
#4014=ORIENTED_EDGE('',*,*,#3147,.T.);
#4015=ORIENTED_EDGE('',*,*,#3125,.F.);
#4016=ORIENTED_EDGE('',*,*,#3122,.F.);
#4017=ORIENTED_EDGE('',*,*,#3118,.T.);
#4018=ORIENTED_EDGE('',*,*,#3131,.F.);
#4019=ORIENTED_EDGE('',*,*,#3089,.F.);
#4020=ORIENTED_EDGE('',*,*,#3093,.T.);
#4021=ORIENTED_EDGE('',*,*,#3136,.F.);
#4022=ORIENTED_EDGE('',*,*,#3149,.F.);
#4023=ORIENTED_EDGE('',*,*,#3150,.T.);
#4024=ORIENTED_EDGE('',*,*,#3149,.T.);
#4025=ORIENTED_EDGE('',*,*,#3135,.F.);
#4026=ORIENTED_EDGE('',*,*,#3095,.F.);
#4027=ORIENTED_EDGE('',*,*,#3091,.T.);
#4028=ORIENTED_EDGE('',*,*,#3134,.F.);
#4029=ORIENTED_EDGE('',*,*,#3107,.F.);
#4030=ORIENTED_EDGE('',*,*,#3111,.T.);
#4031=ORIENTED_EDGE('',*,*,#3128,.F.);
#4032=ORIENTED_EDGE('',*,*,#3151,.F.);
#4033=ORIENTED_EDGE('',*,*,#3047,.T.);
#4034=ORIENTED_EDGE('',*,*,#3068,.T.);
#4035=ORIENTED_EDGE('',*,*,#3152,.T.);
#4036=ORIENTED_EDGE('',*,*,#3151,.T.);
#4037=ORIENTED_EDGE('',*,*,#3127,.F.);
#4038=ORIENTED_EDGE('',*,*,#3113,.F.);
#4039=ORIENTED_EDGE('',*,*,#3109,.T.);
#4040=ORIENTED_EDGE('',*,*,#3133,.F.);
#4041=ORIENTED_EDGE('',*,*,#3104,.F.);
#4042=ORIENTED_EDGE('',*,*,#3100,.T.);
#4043=ORIENTED_EDGE('',*,*,#3130,.F.);
#4044=ORIENTED_EDGE('',*,*,#3146,.F.);
#4045=ORIENTED_EDGE('',*,*,#3152,.F.);
#4046=ORIENTED_EDGE('',*,*,#3145,.F.);
#4047=ORIENTED_EDGE('',*,*,#3148,.F.);
#4048=ORIENTED_EDGE('',*,*,#3150,.F.);
#4049=ORIENTED_EDGE('',*,*,#3066,.T.);
#4050=ORIENTED_EDGE('',*,*,#3087,.T.);
#4051=ORIENTED_EDGE('',*,*,#3137,.T.);
#4052=ORIENTED_EDGE('',*,*,#3139,.T.);
#4053=ORIENTED_EDGE('',*,*,#3141,.T.);
#4054=ORIENTED_EDGE('',*,*,#3143,.T.);
#4055=ORIENTED_EDGE('',*,*,#3153,.F.);
#4056=ORIENTED_EDGE('',*,*,#3154,.F.);
#4057=ORIENTED_EDGE('',*,*,#3155,.F.);
#4058=ORIENTED_EDGE('',*,*,#3156,.F.);
#4059=ORIENTED_EDGE('',*,*,#3157,.F.);
#4060=ORIENTED_EDGE('',*,*,#3154,.T.);
#4061=ORIENTED_EDGE('',*,*,#3158,.F.);
#4062=ORIENTED_EDGE('',*,*,#3159,.F.);
#4063=ORIENTED_EDGE('',*,*,#3160,.F.);
#4064=ORIENTED_EDGE('',*,*,#3161,.T.);
#4065=ORIENTED_EDGE('',*,*,#3162,.F.);
#4066=ORIENTED_EDGE('',*,*,#3163,.F.);
#4067=ORIENTED_EDGE('',*,*,#3164,.F.);
#4068=ORIENTED_EDGE('',*,*,#3165,.F.);
#4069=ORIENTED_EDGE('',*,*,#3161,.F.);
#4070=ORIENTED_EDGE('',*,*,#3166,.F.);
#4071=ORIENTED_EDGE('',*,*,#3167,.T.);
#4072=ORIENTED_EDGE('',*,*,#3168,.F.);
#4073=ORIENTED_EDGE('',*,*,#3169,.F.);
#4074=ORIENTED_EDGE('',*,*,#3170,.F.);
#4075=ORIENTED_EDGE('',*,*,#3171,.F.);
#4076=ORIENTED_EDGE('',*,*,#3167,.F.);
#4077=ORIENTED_EDGE('',*,*,#3172,.F.);
#4078=ORIENTED_EDGE('',*,*,#3173,.T.);
#4079=ORIENTED_EDGE('',*,*,#3174,.F.);
#4080=ORIENTED_EDGE('',*,*,#3175,.F.);
#4081=ORIENTED_EDGE('',*,*,#3176,.F.);
#4082=ORIENTED_EDGE('',*,*,#3177,.F.);
#4083=ORIENTED_EDGE('',*,*,#3173,.F.);
#4084=ORIENTED_EDGE('',*,*,#3156,.T.);
#4085=ORIENTED_EDGE('',*,*,#3178,.T.);
#4086=ORIENTED_EDGE('',*,*,#3176,.T.);
#4087=ORIENTED_EDGE('',*,*,#3179,.T.);
#4088=ORIENTED_EDGE('',*,*,#3170,.T.);
#4089=ORIENTED_EDGE('',*,*,#3180,.T.);
#4090=ORIENTED_EDGE('',*,*,#3164,.T.);
#4091=ORIENTED_EDGE('',*,*,#3181,.T.);
#4092=ORIENTED_EDGE('',*,*,#3182,.T.);
#4093=ORIENTED_EDGE('',*,*,#3183,.F.);
#4094=ORIENTED_EDGE('',*,*,#3184,.T.);
#4095=ORIENTED_EDGE('',*,*,#3159,.T.);
#4096=ORIENTED_EDGE('',*,*,#3184,.F.);
#4097=ORIENTED_EDGE('',*,*,#3185,.F.);
#4098=ORIENTED_EDGE('',*,*,#3186,.T.);
#4099=ORIENTED_EDGE('',*,*,#3162,.T.);
#4100=ORIENTED_EDGE('',*,*,#3186,.F.);
#4101=ORIENTED_EDGE('',*,*,#3187,.F.);
#4102=ORIENTED_EDGE('',*,*,#3188,.T.);
#4103=ORIENTED_EDGE('',*,*,#3168,.T.);
#4104=ORIENTED_EDGE('',*,*,#3188,.F.);
#4105=ORIENTED_EDGE('',*,*,#3189,.F.);
#4106=ORIENTED_EDGE('',*,*,#3190,.T.);
#4107=ORIENTED_EDGE('',*,*,#3174,.T.);
#4108=ORIENTED_EDGE('',*,*,#3190,.F.);
#4109=ORIENTED_EDGE('',*,*,#3191,.F.);
#4110=ORIENTED_EDGE('',*,*,#3192,.T.);
#4111=ORIENTED_EDGE('',*,*,#3193,.T.);
#4112=ORIENTED_EDGE('',*,*,#3192,.F.);
#4113=ORIENTED_EDGE('',*,*,#3193,.F.);
#4114=ORIENTED_EDGE('',*,*,#3194,.F.);
#4115=ORIENTED_EDGE('',*,*,#3182,.F.);
#4116=ORIENTED_EDGE('',*,*,#3195,.T.);
#4117=ORIENTED_EDGE('',*,*,#3194,.T.);
#4118=ORIENTED_EDGE('',*,*,#3195,.F.);
#4119=ORIENTED_EDGE('',*,*,#3153,.T.);
#4120=ORIENTED_EDGE('',*,*,#3181,.F.);
#4121=ORIENTED_EDGE('',*,*,#3163,.T.);
#4122=ORIENTED_EDGE('',*,*,#3160,.T.);
#4123=ORIENTED_EDGE('',*,*,#3165,.T.);
#4124=ORIENTED_EDGE('',*,*,#3180,.F.);
#4125=ORIENTED_EDGE('',*,*,#3169,.T.);
#4126=ORIENTED_EDGE('',*,*,#3166,.T.);
#4127=ORIENTED_EDGE('',*,*,#3171,.T.);
#4128=ORIENTED_EDGE('',*,*,#3179,.F.);
#4129=ORIENTED_EDGE('',*,*,#3175,.T.);
#4130=ORIENTED_EDGE('',*,*,#3172,.T.);
#4131=ORIENTED_EDGE('',*,*,#3177,.T.);
#4132=ORIENTED_EDGE('',*,*,#3178,.F.);
#4133=ORIENTED_EDGE('',*,*,#3155,.T.);
#4134=ORIENTED_EDGE('',*,*,#3157,.T.);
#4135=ORIENTED_EDGE('',*,*,#3196,.T.);
#4136=ORIENTED_EDGE('',*,*,#3197,.T.);
#4137=ORIENTED_EDGE('',*,*,#3196,.F.);
#4138=ORIENTED_EDGE('',*,*,#3158,.T.);
#4139=ORIENTED_EDGE('',*,*,#3197,.F.);
#4140=ORIENTED_EDGE('',*,*,#3191,.T.);
#4141=ORIENTED_EDGE('',*,*,#3189,.T.);
#4142=ORIENTED_EDGE('',*,*,#3187,.T.);
#4143=ORIENTED_EDGE('',*,*,#3185,.T.);
#4144=ORIENTED_EDGE('',*,*,#3183,.T.);
#4145=ORIENTED_EDGE('',*,*,#3198,.F.);
#4146=ORIENTED_EDGE('',*,*,#3199,.F.);
#4147=ORIENTED_EDGE('',*,*,#3200,.F.);
#4148=ORIENTED_EDGE('',*,*,#3201,.F.);
#4149=ORIENTED_EDGE('',*,*,#3202,.F.);
#4150=ORIENTED_EDGE('',*,*,#3199,.T.);
#4151=ORIENTED_EDGE('',*,*,#3203,.F.);
#4152=ORIENTED_EDGE('',*,*,#3204,.F.);
#4153=ORIENTED_EDGE('',*,*,#3205,.F.);
#4154=ORIENTED_EDGE('',*,*,#3206,.T.);
#4155=ORIENTED_EDGE('',*,*,#3207,.F.);
#4156=ORIENTED_EDGE('',*,*,#3208,.F.);
#4157=ORIENTED_EDGE('',*,*,#3209,.F.);
#4158=ORIENTED_EDGE('',*,*,#3210,.F.);
#4159=ORIENTED_EDGE('',*,*,#3206,.F.);
#4160=ORIENTED_EDGE('',*,*,#3211,.F.);
#4161=ORIENTED_EDGE('',*,*,#3212,.T.);
#4162=ORIENTED_EDGE('',*,*,#3213,.F.);
#4163=ORIENTED_EDGE('',*,*,#3214,.F.);
#4164=ORIENTED_EDGE('',*,*,#3215,.F.);
#4165=ORIENTED_EDGE('',*,*,#3216,.F.);
#4166=ORIENTED_EDGE('',*,*,#3212,.F.);
#4167=ORIENTED_EDGE('',*,*,#3217,.F.);
#4168=ORIENTED_EDGE('',*,*,#3218,.T.);
#4169=ORIENTED_EDGE('',*,*,#3219,.F.);
#4170=ORIENTED_EDGE('',*,*,#3220,.F.);
#4171=ORIENTED_EDGE('',*,*,#3221,.F.);
#4172=ORIENTED_EDGE('',*,*,#3222,.F.);
#4173=ORIENTED_EDGE('',*,*,#3218,.F.);
#4174=ORIENTED_EDGE('',*,*,#3201,.T.);
#4175=ORIENTED_EDGE('',*,*,#3223,.T.);
#4176=ORIENTED_EDGE('',*,*,#3221,.T.);
#4177=ORIENTED_EDGE('',*,*,#3224,.T.);
#4178=ORIENTED_EDGE('',*,*,#3215,.T.);
#4179=ORIENTED_EDGE('',*,*,#3225,.T.);
#4180=ORIENTED_EDGE('',*,*,#3209,.T.);
#4181=ORIENTED_EDGE('',*,*,#3226,.T.);
#4182=ORIENTED_EDGE('',*,*,#3227,.T.);
#4183=ORIENTED_EDGE('',*,*,#3228,.F.);
#4184=ORIENTED_EDGE('',*,*,#3229,.T.);
#4185=ORIENTED_EDGE('',*,*,#3204,.T.);
#4186=ORIENTED_EDGE('',*,*,#3229,.F.);
#4187=ORIENTED_EDGE('',*,*,#3230,.F.);
#4188=ORIENTED_EDGE('',*,*,#3231,.T.);
#4189=ORIENTED_EDGE('',*,*,#3207,.T.);
#4190=ORIENTED_EDGE('',*,*,#3231,.F.);
#4191=ORIENTED_EDGE('',*,*,#3232,.F.);
#4192=ORIENTED_EDGE('',*,*,#3233,.T.);
#4193=ORIENTED_EDGE('',*,*,#3213,.T.);
#4194=ORIENTED_EDGE('',*,*,#3233,.F.);
#4195=ORIENTED_EDGE('',*,*,#3234,.F.);
#4196=ORIENTED_EDGE('',*,*,#3235,.T.);
#4197=ORIENTED_EDGE('',*,*,#3219,.T.);
#4198=ORIENTED_EDGE('',*,*,#3235,.F.);
#4199=ORIENTED_EDGE('',*,*,#3236,.F.);
#4200=ORIENTED_EDGE('',*,*,#3237,.T.);
#4201=ORIENTED_EDGE('',*,*,#3238,.T.);
#4202=ORIENTED_EDGE('',*,*,#3237,.F.);
#4203=ORIENTED_EDGE('',*,*,#3238,.F.);
#4204=ORIENTED_EDGE('',*,*,#3239,.F.);
#4205=ORIENTED_EDGE('',*,*,#3227,.F.);
#4206=ORIENTED_EDGE('',*,*,#3240,.T.);
#4207=ORIENTED_EDGE('',*,*,#3239,.T.);
#4208=ORIENTED_EDGE('',*,*,#3240,.F.);
#4209=ORIENTED_EDGE('',*,*,#3198,.T.);
#4210=ORIENTED_EDGE('',*,*,#3226,.F.);
#4211=ORIENTED_EDGE('',*,*,#3208,.T.);
#4212=ORIENTED_EDGE('',*,*,#3205,.T.);
#4213=ORIENTED_EDGE('',*,*,#3210,.T.);
#4214=ORIENTED_EDGE('',*,*,#3225,.F.);
#4215=ORIENTED_EDGE('',*,*,#3214,.T.);
#4216=ORIENTED_EDGE('',*,*,#3211,.T.);
#4217=ORIENTED_EDGE('',*,*,#3216,.T.);
#4218=ORIENTED_EDGE('',*,*,#3224,.F.);
#4219=ORIENTED_EDGE('',*,*,#3220,.T.);
#4220=ORIENTED_EDGE('',*,*,#3217,.T.);
#4221=ORIENTED_EDGE('',*,*,#3222,.T.);
#4222=ORIENTED_EDGE('',*,*,#3223,.F.);
#4223=ORIENTED_EDGE('',*,*,#3200,.T.);
#4224=ORIENTED_EDGE('',*,*,#3202,.T.);
#4225=ORIENTED_EDGE('',*,*,#3241,.T.);
#4226=ORIENTED_EDGE('',*,*,#3242,.T.);
#4227=ORIENTED_EDGE('',*,*,#3241,.F.);
#4228=ORIENTED_EDGE('',*,*,#3203,.T.);
#4229=ORIENTED_EDGE('',*,*,#3242,.F.);
#4230=ORIENTED_EDGE('',*,*,#3236,.T.);
#4231=ORIENTED_EDGE('',*,*,#3234,.T.);
#4232=ORIENTED_EDGE('',*,*,#3232,.T.);
#4233=ORIENTED_EDGE('',*,*,#3230,.T.);
#4234=ORIENTED_EDGE('',*,*,#3228,.T.);
#4235=ORIENTED_EDGE('',*,*,#3243,.F.);
#4236=ORIENTED_EDGE('',*,*,#3244,.F.);
#4237=ORIENTED_EDGE('',*,*,#3245,.T.);
#4238=ORIENTED_EDGE('',*,*,#3243,.T.);
#4239=ORIENTED_EDGE('',*,*,#3245,.F.);
#4240=ORIENTED_EDGE('',*,*,#3246,.F.);
#4241=ORIENTED_EDGE('',*,*,#3247,.T.);
#4242=ORIENTED_EDGE('',*,*,#3244,.T.);
#4243=ORIENTED_EDGE('',*,*,#3247,.F.);
#4244=ORIENTED_EDGE('',*,*,#3248,.F.);
#4245=ORIENTED_EDGE('',*,*,#3249,.T.);
#4246=ORIENTED_EDGE('',*,*,#3246,.T.);
#4247=ORIENTED_EDGE('',*,*,#3249,.F.);
#4248=ORIENTED_EDGE('',*,*,#3248,.T.);
#4249=ORIENTED_EDGE('',*,*,#3250,.F.);
#4250=ORIENTED_EDGE('',*,*,#3251,.F.);
#4251=ORIENTED_EDGE('',*,*,#3252,.T.);
#4252=ORIENTED_EDGE('',*,*,#3250,.T.);
#4253=ORIENTED_EDGE('',*,*,#3252,.F.);
#4254=ORIENTED_EDGE('',*,*,#3253,.F.);
#4255=ORIENTED_EDGE('',*,*,#3254,.T.);
#4256=ORIENTED_EDGE('',*,*,#3251,.T.);
#4257=ORIENTED_EDGE('',*,*,#3254,.F.);
#4258=ORIENTED_EDGE('',*,*,#3255,.F.);
#4259=ORIENTED_EDGE('',*,*,#3256,.T.);
#4260=ORIENTED_EDGE('',*,*,#3253,.T.);
#4261=ORIENTED_EDGE('',*,*,#3256,.F.);
#4262=ORIENTED_EDGE('',*,*,#3255,.T.);
#4263=ORIENTED_EDGE('',*,*,#3257,.T.);
#4264=ORIENTED_EDGE('',*,*,#3258,.T.);
#4265=ORIENTED_EDGE('',*,*,#3259,.T.);
#4266=ORIENTED_EDGE('',*,*,#3260,.F.);
#4267=ORIENTED_EDGE('',*,*,#3261,.T.);
#4268=ORIENTED_EDGE('',*,*,#3262,.T.);
#4269=ORIENTED_EDGE('',*,*,#3263,.T.);
#4270=ORIENTED_EDGE('',*,*,#3258,.F.);
#4271=ORIENTED_EDGE('',*,*,#3264,.T.);
#4272=ORIENTED_EDGE('',*,*,#3265,.T.);
#4273=ORIENTED_EDGE('',*,*,#3266,.T.);
#4274=ORIENTED_EDGE('',*,*,#3262,.F.);
#4275=ORIENTED_EDGE('',*,*,#3267,.T.);
#4276=ORIENTED_EDGE('',*,*,#3268,.T.);
#4277=ORIENTED_EDGE('',*,*,#3269,.T.);
#4278=ORIENTED_EDGE('',*,*,#3265,.F.);
#4279=ORIENTED_EDGE('',*,*,#3270,.T.);
#4280=ORIENTED_EDGE('',*,*,#3271,.T.);
#4281=ORIENTED_EDGE('',*,*,#3272,.T.);
#4282=ORIENTED_EDGE('',*,*,#3268,.F.);
#4283=ORIENTED_EDGE('',*,*,#3273,.T.);
#4284=ORIENTED_EDGE('',*,*,#3260,.T.);
#4285=ORIENTED_EDGE('',*,*,#3274,.T.);
#4286=ORIENTED_EDGE('',*,*,#3271,.F.);
#4287=ORIENTED_EDGE('',*,*,#3273,.F.);
#4288=ORIENTED_EDGE('',*,*,#3270,.F.);
#4289=ORIENTED_EDGE('',*,*,#3267,.F.);
#4290=ORIENTED_EDGE('',*,*,#3264,.F.);
#4291=ORIENTED_EDGE('',*,*,#3261,.F.);
#4292=ORIENTED_EDGE('',*,*,#3257,.F.);
#4293=ORIENTED_EDGE('',*,*,#3274,.F.);
#4294=ORIENTED_EDGE('',*,*,#3259,.F.);
#4295=ORIENTED_EDGE('',*,*,#3263,.F.);
#4296=ORIENTED_EDGE('',*,*,#3266,.F.);
#4297=ORIENTED_EDGE('',*,*,#3269,.F.);
#4298=ORIENTED_EDGE('',*,*,#3272,.F.);
#4299=ORIENTED_EDGE('',*,*,#3275,.F.);
#4300=ORIENTED_EDGE('',*,*,#3276,.F.);
#4301=ORIENTED_EDGE('',*,*,#3277,.T.);
#4302=ORIENTED_EDGE('',*,*,#3278,.F.);
#4303=ORIENTED_EDGE('',*,*,#3279,.F.);
#4304=ORIENTED_EDGE('',*,*,#3277,.F.);
#4305=ORIENTED_EDGE('',*,*,#3278,.T.);
#4306=ORIENTED_EDGE('',*,*,#3279,.T.);
#4307=ORIENTED_EDGE('',*,*,#3280,.T.);
#4308=ORIENTED_EDGE('',*,*,#3281,.T.);
#4309=ORIENTED_EDGE('',*,*,#3280,.F.);
#4310=ORIENTED_EDGE('',*,*,#3282,.T.);
#4311=ORIENTED_EDGE('',*,*,#3283,.T.);
#4312=ORIENTED_EDGE('',*,*,#3284,.F.);
#4313=ORIENTED_EDGE('',*,*,#3283,.F.);
#4314=ORIENTED_EDGE('',*,*,#3284,.T.);
#4315=ORIENTED_EDGE('',*,*,#3285,.T.);
#4316=ORIENTED_EDGE('',*,*,#3286,.F.);
#4317=ORIENTED_EDGE('',*,*,#3285,.F.);
#4318=ORIENTED_EDGE('',*,*,#3281,.F.);
#4319=ORIENTED_EDGE('',*,*,#3286,.T.);
#4320=ORIENTED_EDGE('',*,*,#3287,.F.);
#4321=ORIENTED_EDGE('',*,*,#3288,.T.);
#4322=ORIENTED_EDGE('',*,*,#3275,.T.);
#4323=ORIENTED_EDGE('',*,*,#3276,.T.);
#4324=ORIENTED_EDGE('',*,*,#3288,.F.);
#4325=ORIENTED_EDGE('',*,*,#3287,.T.);
#4326=ORIENTED_EDGE('',*,*,#3289,.F.);
#4327=ORIENTED_EDGE('',*,*,#3289,.T.);
#4328=ORIENTED_EDGE('',*,*,#3290,.T.);
#4329=ORIENTED_EDGE('',*,*,#3282,.F.);
#4330=ORIENTED_EDGE('',*,*,#3290,.F.);
#4331=ORIENTED_EDGE('',*,*,#3291,.F.);
#4332=ORIENTED_EDGE('',*,*,#3292,.F.);
#4333=ORIENTED_EDGE('',*,*,#3293,.T.);
#4334=ORIENTED_EDGE('',*,*,#3294,.F.);
#4335=ORIENTED_EDGE('',*,*,#3295,.F.);
#4336=ORIENTED_EDGE('',*,*,#3293,.F.);
#4337=ORIENTED_EDGE('',*,*,#3296,.T.);
#4338=ORIENTED_EDGE('',*,*,#3297,.T.);
#4339=ORIENTED_EDGE('',*,*,#3294,.T.);
#4340=ORIENTED_EDGE('',*,*,#3295,.T.);
#4341=ORIENTED_EDGE('',*,*,#3297,.F.);
#4342=ORIENTED_EDGE('',*,*,#3298,.F.);
#4343=ORIENTED_EDGE('',*,*,#3299,.T.);
#4344=ORIENTED_EDGE('',*,*,#3300,.F.);
#4345=ORIENTED_EDGE('',*,*,#3301,.T.);
#4346=ORIENTED_EDGE('',*,*,#3298,.T.);
#4347=ORIENTED_EDGE('',*,*,#3301,.F.);
#4348=ORIENTED_EDGE('',*,*,#3302,.F.);
#4349=ORIENTED_EDGE('',*,*,#3303,.T.);
#4350=ORIENTED_EDGE('',*,*,#3300,.T.);
#4351=ORIENTED_EDGE('',*,*,#3303,.F.);
#4352=ORIENTED_EDGE('',*,*,#3304,.F.);
#4353=ORIENTED_EDGE('',*,*,#3305,.T.);
#4354=ORIENTED_EDGE('',*,*,#3302,.T.);
#4355=ORIENTED_EDGE('',*,*,#3305,.F.);
#4356=ORIENTED_EDGE('',*,*,#3304,.T.);
#4357=ORIENTED_EDGE('',*,*,#3296,.F.);
#4358=ORIENTED_EDGE('',*,*,#3291,.T.);
#4359=ORIENTED_EDGE('',*,*,#3292,.T.);
#4360=ORIENTED_EDGE('',*,*,#3306,.T.);
#4361=ORIENTED_EDGE('',*,*,#3299,.F.);
#4362=ORIENTED_EDGE('',*,*,#3306,.F.);
#4363=ORIENTED_EDGE('',*,*,#3307,.T.);
#4364=ORIENTED_EDGE('',*,*,#3307,.F.);
#4365=ORIENTED_EDGE('',*,*,#3308,.T.);
#4366=ORIENTED_EDGE('',*,*,#3308,.F.);
#4367=ORIENTED_EDGE('',*,*,#3309,.T.);
#4368=ORIENTED_EDGE('',*,*,#3309,.F.);
#4369=ORIENTED_EDGE('',*,*,#3310,.T.);
#4370=ORIENTED_EDGE('',*,*,#3310,.F.);
#4371=ORIENTED_EDGE('',*,*,#3311,.T.);
#4372=ORIENTED_EDGE('',*,*,#3311,.F.);
#4373=ORIENTED_EDGE('',*,*,#3312,.T.);
#4374=ORIENTED_EDGE('',*,*,#3312,.F.);
#4375=ORIENTED_EDGE('',*,*,#3313,.T.);
#4376=ORIENTED_EDGE('',*,*,#3313,.F.);
#4377=ORIENTED_EDGE('',*,*,#3314,.T.);
#4378=ORIENTED_EDGE('',*,*,#3314,.F.);
#4379=ORIENTED_EDGE('',*,*,#3315,.F.);
#4380=ORIENTED_EDGE('',*,*,#3316,.F.);
#4381=ORIENTED_EDGE('',*,*,#3317,.F.);
#4382=ORIENTED_EDGE('',*,*,#3318,.F.);
#4383=ORIENTED_EDGE('',*,*,#3317,.T.);
#4384=ORIENTED_EDGE('',*,*,#3319,.F.);
#4385=ORIENTED_EDGE('',*,*,#3320,.T.);
#4386=ORIENTED_EDGE('',*,*,#3321,.F.);
#4387=ORIENTED_EDGE('',*,*,#3322,.T.);
#4388=ORIENTED_EDGE('',*,*,#3323,.F.);
#4389=ORIENTED_EDGE('',*,*,#3324,.T.);
#4390=ORIENTED_EDGE('',*,*,#3325,.T.);
#4391=ORIENTED_EDGE('',*,*,#3326,.F.);
#4392=ORIENTED_EDGE('',*,*,#3325,.F.);
#4393=ORIENTED_EDGE('',*,*,#3327,.T.);
#4394=ORIENTED_EDGE('',*,*,#3328,.F.);
#4395=ORIENTED_EDGE('',*,*,#3329,.T.);
#4396=ORIENTED_EDGE('',*,*,#3330,.F.);
#4397=ORIENTED_EDGE('',*,*,#3331,.T.);
#4398=ORIENTED_EDGE('',*,*,#3332,.F.);
#4399=ORIENTED_EDGE('',*,*,#3333,.T.);
#4400=ORIENTED_EDGE('',*,*,#3334,.F.);
#4401=ORIENTED_EDGE('',*,*,#3335,.T.);
#4402=ORIENTED_EDGE('',*,*,#3336,.F.);
#4403=ORIENTED_EDGE('',*,*,#3316,.T.);
#4404=ORIENTED_EDGE('',*,*,#3337,.T.);
#4405=ORIENTED_EDGE('',*,*,#3338,.T.);
#4406=ORIENTED_EDGE('',*,*,#3319,.T.);
#4407=ORIENTED_EDGE('',*,*,#3339,.F.);
#4408=ORIENTED_EDGE('',*,*,#3340,.F.);
#4409=ORIENTED_EDGE('',*,*,#3320,.F.);
#4410=ORIENTED_EDGE('',*,*,#3338,.F.);
#4411=ORIENTED_EDGE('',*,*,#3340,.T.);
#4412=ORIENTED_EDGE('',*,*,#3341,.T.);
#4413=ORIENTED_EDGE('',*,*,#3342,.T.);
#4414=ORIENTED_EDGE('',*,*,#3321,.T.);
#4415=ORIENTED_EDGE('',*,*,#3343,.F.);
#4416=ORIENTED_EDGE('',*,*,#3344,.F.);
#4417=ORIENTED_EDGE('',*,*,#3322,.F.);
#4418=ORIENTED_EDGE('',*,*,#3342,.F.);
#4419=ORIENTED_EDGE('',*,*,#3344,.T.);
#4420=ORIENTED_EDGE('',*,*,#3345,.T.);
#4421=ORIENTED_EDGE('',*,*,#3346,.T.);
#4422=ORIENTED_EDGE('',*,*,#3323,.T.);
#4423=ORIENTED_EDGE('',*,*,#3347,.F.);
#4424=ORIENTED_EDGE('',*,*,#3348,.F.);
#4425=ORIENTED_EDGE('',*,*,#3327,.F.);
#4426=ORIENTED_EDGE('',*,*,#3324,.F.);
#4427=ORIENTED_EDGE('',*,*,#3346,.F.);
#4428=ORIENTED_EDGE('',*,*,#3349,.F.);
#4429=ORIENTED_EDGE('',*,*,#3348,.T.);
#4430=ORIENTED_EDGE('',*,*,#3350,.T.);
#4431=ORIENTED_EDGE('',*,*,#3351,.T.);
#4432=ORIENTED_EDGE('',*,*,#3328,.T.);
#4433=ORIENTED_EDGE('',*,*,#3352,.F.);
#4434=ORIENTED_EDGE('',*,*,#3353,.F.);
#4435=ORIENTED_EDGE('',*,*,#3329,.F.);
#4436=ORIENTED_EDGE('',*,*,#3351,.F.);
#4437=ORIENTED_EDGE('',*,*,#3353,.T.);
#4438=ORIENTED_EDGE('',*,*,#3354,.T.);
#4439=ORIENTED_EDGE('',*,*,#3355,.T.);
#4440=ORIENTED_EDGE('',*,*,#3330,.T.);
#4441=ORIENTED_EDGE('',*,*,#3356,.F.);
#4442=ORIENTED_EDGE('',*,*,#3357,.F.);
#4443=ORIENTED_EDGE('',*,*,#3331,.F.);
#4444=ORIENTED_EDGE('',*,*,#3355,.F.);
#4445=ORIENTED_EDGE('',*,*,#3357,.T.);
#4446=ORIENTED_EDGE('',*,*,#3358,.T.);
#4447=ORIENTED_EDGE('',*,*,#3359,.T.);
#4448=ORIENTED_EDGE('',*,*,#3332,.T.);
#4449=ORIENTED_EDGE('',*,*,#3333,.F.);
#4450=ORIENTED_EDGE('',*,*,#3359,.F.);
#4451=ORIENTED_EDGE('',*,*,#3360,.F.);
#4452=ORIENTED_EDGE('',*,*,#3361,.F.);
#4453=ORIENTED_EDGE('',*,*,#3362,.F.);
#4454=ORIENTED_EDGE('',*,*,#3363,.T.);
#4455=ORIENTED_EDGE('',*,*,#3349,.T.);
#4456=ORIENTED_EDGE('',*,*,#3345,.F.);
#4457=ORIENTED_EDGE('',*,*,#3343,.T.);
#4458=ORIENTED_EDGE('',*,*,#3341,.F.);
#4459=ORIENTED_EDGE('',*,*,#3339,.T.);
#4460=ORIENTED_EDGE('',*,*,#3337,.F.);
#4461=ORIENTED_EDGE('',*,*,#3315,.T.);
#4462=ORIENTED_EDGE('',*,*,#3364,.F.);
#4463=ORIENTED_EDGE('',*,*,#3365,.T.);
#4464=ORIENTED_EDGE('',*,*,#3366,.F.);
#4465=ORIENTED_EDGE('',*,*,#3360,.T.);
#4466=ORIENTED_EDGE('',*,*,#3358,.F.);
#4467=ORIENTED_EDGE('',*,*,#3356,.T.);
#4468=ORIENTED_EDGE('',*,*,#3354,.F.);
#4469=ORIENTED_EDGE('',*,*,#3352,.T.);
#4470=ORIENTED_EDGE('',*,*,#3350,.F.);
#4471=ORIENTED_EDGE('',*,*,#3347,.T.);
#4472=ORIENTED_EDGE('',*,*,#3363,.F.);
#4473=ORIENTED_EDGE('',*,*,#3318,.T.);
#4474=ORIENTED_EDGE('',*,*,#3336,.T.);
#4475=ORIENTED_EDGE('',*,*,#3367,.T.);
#4476=ORIENTED_EDGE('',*,*,#3364,.T.);
#4477=ORIENTED_EDGE('',*,*,#3335,.F.);
#4478=ORIENTED_EDGE('',*,*,#3368,.F.);
#4479=ORIENTED_EDGE('',*,*,#3365,.F.);
#4480=ORIENTED_EDGE('',*,*,#3367,.F.);
#4481=ORIENTED_EDGE('',*,*,#3326,.T.);
#4482=ORIENTED_EDGE('',*,*,#3362,.T.);
#4483=ORIENTED_EDGE('',*,*,#3361,.T.);
#4484=ORIENTED_EDGE('',*,*,#3366,.T.);
#4485=ORIENTED_EDGE('',*,*,#3368,.T.);
#4486=ORIENTED_EDGE('',*,*,#3334,.T.);
#4487=ORIENTED_EDGE('',*,*,#3369,.F.);
#4488=ORIENTED_EDGE('',*,*,#3370,.T.);
#4489=ORIENTED_EDGE('',*,*,#3371,.F.);
#4490=ORIENTED_EDGE('',*,*,#3372,.T.);
#4491=ORIENTED_EDGE('',*,*,#3369,.T.);
#4492=ORIENTED_EDGE('',*,*,#3372,.F.);
#4493=ORIENTED_EDGE('',*,*,#3371,.T.);
#4494=ORIENTED_EDGE('',*,*,#3373,.F.);
#4495=ORIENTED_EDGE('',*,*,#3373,.T.);
#4496=ORIENTED_EDGE('',*,*,#3374,.T.);
#4497=ORIENTED_EDGE('',*,*,#3370,.F.);
#4498=ORIENTED_EDGE('',*,*,#3374,.F.);
#4499=ORIENTED_EDGE('',*,*,#3375,.F.);
#4500=ORIENTED_EDGE('',*,*,#3376,.T.);
#4501=ORIENTED_EDGE('',*,*,#3377,.F.);
#4502=ORIENTED_EDGE('',*,*,#3378,.T.);
#4503=ORIENTED_EDGE('',*,*,#3375,.T.);
#4504=ORIENTED_EDGE('',*,*,#3378,.F.);
#4505=ORIENTED_EDGE('',*,*,#3377,.T.);
#4506=ORIENTED_EDGE('',*,*,#3379,.F.);
#4507=ORIENTED_EDGE('',*,*,#3379,.T.);
#4508=ORIENTED_EDGE('',*,*,#3380,.T.);
#4509=ORIENTED_EDGE('',*,*,#3376,.F.);
#4510=ORIENTED_EDGE('',*,*,#3380,.F.);
#4511=ORIENTED_EDGE('',*,*,#3381,.F.);
#4512=ORIENTED_EDGE('',*,*,#3382,.T.);
#4513=ORIENTED_EDGE('',*,*,#3383,.F.);
#4514=ORIENTED_EDGE('',*,*,#3382,.F.);
#4515=ORIENTED_EDGE('',*,*,#3381,.T.);
#4516=ORIENTED_EDGE('',*,*,#3384,.F.);
#4517=ORIENTED_EDGE('',*,*,#3385,.T.);
#4518=ORIENTED_EDGE('',*,*,#3386,.F.);
#4519=ORIENTED_EDGE('',*,*,#3385,.F.);
#4520=ORIENTED_EDGE('',*,*,#3387,.T.);
#4521=ORIENTED_EDGE('',*,*,#3388,.F.);
#4522=ORIENTED_EDGE('',*,*,#3389,.F.);
#4523=ORIENTED_EDGE('',*,*,#3390,.T.);
#4524=ORIENTED_EDGE('',*,*,#3391,.F.);
#4525=ORIENTED_EDGE('',*,*,#3392,.F.);
#4526=ORIENTED_EDGE('',*,*,#3393,.F.);
#4527=ORIENTED_EDGE('',*,*,#3394,.F.);
#4528=ORIENTED_EDGE('',*,*,#3395,.F.);
#4529=ORIENTED_EDGE('',*,*,#3396,.F.);
#4530=ORIENTED_EDGE('',*,*,#3397,.F.);
#4531=ORIENTED_EDGE('',*,*,#3390,.F.);
#4532=ORIENTED_EDGE('',*,*,#3384,.T.);
#4533=ORIENTED_EDGE('',*,*,#3398,.T.);
#4534=ORIENTED_EDGE('',*,*,#3399,.F.);
#4535=ORIENTED_EDGE('',*,*,#3400,.F.);
#4536=ORIENTED_EDGE('',*,*,#3387,.F.);
#4537=ORIENTED_EDGE('',*,*,#3397,.T.);
#4538=ORIENTED_EDGE('',*,*,#3401,.F.);
#4539=ORIENTED_EDGE('',*,*,#3391,.T.);
#4540=ORIENTED_EDGE('',*,*,#3389,.T.);
#4541=ORIENTED_EDGE('',*,*,#3402,.F.);
#4542=ORIENTED_EDGE('',*,*,#3403,.F.);
#4543=ORIENTED_EDGE('',*,*,#3404,.F.);
#4544=ORIENTED_EDGE('',*,*,#3405,.F.);
#4545=ORIENTED_EDGE('',*,*,#3393,.T.);
#4546=ORIENTED_EDGE('',*,*,#3406,.F.);
#4547=ORIENTED_EDGE('',*,*,#3395,.T.);
#4548=ORIENTED_EDGE('',*,*,#3407,.T.);
#4549=ORIENTED_EDGE('',*,*,#3408,.F.);
#4550=ORIENTED_EDGE('',*,*,#3394,.T.);
#4551=ORIENTED_EDGE('',*,*,#3405,.T.);
#4552=ORIENTED_EDGE('',*,*,#3409,.F.);
#4553=ORIENTED_EDGE('',*,*,#3407,.F.);
#4554=ORIENTED_EDGE('',*,*,#3400,.T.);
#4555=ORIENTED_EDGE('',*,*,#3410,.T.);
#4556=ORIENTED_EDGE('',*,*,#3408,.T.);
#4557=ORIENTED_EDGE('',*,*,#3409,.T.);
#4558=ORIENTED_EDGE('',*,*,#3404,.T.);
#4559=ORIENTED_EDGE('',*,*,#3411,.T.);
#4560=ORIENTED_EDGE('',*,*,#3402,.T.);
#4561=ORIENTED_EDGE('',*,*,#3388,.T.);
#4562=ORIENTED_EDGE('',*,*,#3386,.T.);
#4563=ORIENTED_EDGE('',*,*,#3412,.F.);
#4564=ORIENTED_EDGE('',*,*,#3403,.T.);
#4565=ORIENTED_EDGE('',*,*,#3392,.T.);
#4566=ORIENTED_EDGE('',*,*,#3401,.T.);
#4567=ORIENTED_EDGE('',*,*,#3411,.F.);
#4568=ORIENTED_EDGE('',*,*,#3406,.T.);
#4569=ORIENTED_EDGE('',*,*,#3410,.F.);
#4570=ORIENTED_EDGE('',*,*,#3399,.T.);
#4571=ORIENTED_EDGE('',*,*,#3396,.T.);
#4572=ORIENTED_EDGE('',*,*,#3413,.F.);
#4573=ORIENTED_EDGE('',*,*,#3414,.F.);
#4574=ORIENTED_EDGE('',*,*,#3398,.F.);
#4575=ORIENTED_EDGE('',*,*,#3415,.T.);
#4576=ORIENTED_EDGE('',*,*,#3413,.T.);
#4577=ORIENTED_EDGE('',*,*,#3415,.F.);
#4578=ORIENTED_EDGE('',*,*,#3414,.T.);
#4579=ORIENTED_EDGE('',*,*,#3416,.T.);
#4580=ORIENTED_EDGE('',*,*,#3417,.T.);
#4581=ORIENTED_EDGE('',*,*,#3416,.F.);
#4582=ORIENTED_EDGE('',*,*,#3418,.F.);
#4583=ORIENTED_EDGE('',*,*,#3419,.T.);
#4584=ORIENTED_EDGE('',*,*,#3412,.T.);
#4585=ORIENTED_EDGE('',*,*,#3419,.F.);
#4586=ORIENTED_EDGE('',*,*,#3418,.T.);
#4587=ORIENTED_EDGE('',*,*,#3383,.T.);
#4588=ORIENTED_EDGE('',*,*,#3417,.F.);
#4589=ORIENTED_EDGE('',*,*,#3420,.F.);
#4590=ORIENTED_EDGE('',*,*,#3421,.T.);
#4591=ORIENTED_EDGE('',*,*,#3422,.T.);
#4592=ORIENTED_EDGE('',*,*,#3421,.F.);
#4593=ORIENTED_EDGE('',*,*,#3423,.F.);
#4594=ORIENTED_EDGE('',*,*,#3424,.T.);
#4595=ORIENTED_EDGE('',*,*,#3425,.T.);
#4596=ORIENTED_EDGE('',*,*,#3424,.F.);
#4597=ORIENTED_EDGE('',*,*,#3423,.T.);
#4598=ORIENTED_EDGE('',*,*,#3420,.T.);
#4599=ORIENTED_EDGE('',*,*,#3425,.F.);
#4600=ORIENTED_EDGE('',*,*,#3422,.F.);
#4601=ORIENTED_EDGE('',*,*,#3426,.F.);
#4602=ORIENTED_EDGE('',*,*,#3427,.F.);
#4603=ORIENTED_EDGE('',*,*,#3428,.F.);
#4604=ORIENTED_EDGE('',*,*,#3429,.F.);
#4605=ORIENTED_EDGE('',*,*,#3430,.T.);
#4606=ORIENTED_EDGE('',*,*,#3427,.T.);
#4607=ORIENTED_EDGE('',*,*,#3431,.F.);
#4608=ORIENTED_EDGE('',*,*,#3432,.T.);
#4609=ORIENTED_EDGE('',*,*,#3433,.F.);
#4610=ORIENTED_EDGE('',*,*,#3428,.T.);
#4611=ORIENTED_EDGE('',*,*,#3430,.F.);
#4612=ORIENTED_EDGE('',*,*,#3434,.F.);
#4613=ORIENTED_EDGE('',*,*,#3432,.F.);
#4614=ORIENTED_EDGE('',*,*,#3435,.F.);
#4615=ORIENTED_EDGE('',*,*,#3436,.F.);
#4616=ORIENTED_EDGE('',*,*,#3437,.F.);
#4617=ORIENTED_EDGE('',*,*,#3438,.F.);
#4618=ORIENTED_EDGE('',*,*,#3439,.F.);
#4619=ORIENTED_EDGE('',*,*,#3440,.T.);
#4620=ORIENTED_EDGE('',*,*,#3441,.F.);
#4621=ORIENTED_EDGE('',*,*,#3442,.T.);
#4622=ORIENTED_EDGE('',*,*,#3443,.F.);
#4623=ORIENTED_EDGE('',*,*,#3444,.F.);
#4624=ORIENTED_EDGE('',*,*,#3436,.T.);
#4625=ORIENTED_EDGE('',*,*,#3445,.F.);
#4626=ORIENTED_EDGE('',*,*,#3440,.F.);
#4627=ORIENTED_EDGE('',*,*,#3446,.F.);
#4628=ORIENTED_EDGE('',*,*,#3442,.F.);
#4629=ORIENTED_EDGE('',*,*,#3447,.F.);
#4630=ORIENTED_EDGE('',*,*,#3448,.T.);
#4631=ORIENTED_EDGE('',*,*,#3445,.T.);
#4632=ORIENTED_EDGE('',*,*,#3435,.T.);
#4633=ORIENTED_EDGE('',*,*,#3444,.T.);
#4634=ORIENTED_EDGE('',*,*,#3449,.T.);
#4635=ORIENTED_EDGE('',*,*,#3450,.T.);
#4636=ORIENTED_EDGE('',*,*,#3449,.F.);
#4637=ORIENTED_EDGE('',*,*,#3443,.T.);
#4638=ORIENTED_EDGE('',*,*,#3446,.T.);
#4639=ORIENTED_EDGE('',*,*,#3441,.T.);
#4640=ORIENTED_EDGE('',*,*,#3448,.F.);
#4641=ORIENTED_EDGE('',*,*,#3433,.T.);
#4642=ORIENTED_EDGE('',*,*,#3434,.T.);
#4643=ORIENTED_EDGE('',*,*,#3431,.T.);
#4644=ORIENTED_EDGE('',*,*,#3426,.T.);
#4645=ORIENTED_EDGE('',*,*,#3451,.F.);
#4646=ORIENTED_EDGE('',*,*,#3452,.T.);
#4647=ORIENTED_EDGE('',*,*,#3439,.T.);
#4648=ORIENTED_EDGE('',*,*,#3453,.T.);
#4649=ORIENTED_EDGE('',*,*,#3454,.T.);
#4650=ORIENTED_EDGE('',*,*,#3453,.F.);
#4651=ORIENTED_EDGE('',*,*,#3438,.T.);
#4652=ORIENTED_EDGE('',*,*,#3437,.T.);
#4653=ORIENTED_EDGE('',*,*,#3452,.F.);
#4654=ORIENTED_EDGE('',*,*,#3429,.T.);
#4655=ORIENTED_EDGE('',*,*,#3451,.T.);
#4656=ORIENTED_EDGE('',*,*,#3447,.T.);
#4657=ORIENTED_EDGE('',*,*,#3454,.F.);
#4658=ORIENTED_EDGE('',*,*,#3450,.F.);
#4659=ORIENTED_EDGE('',*,*,#3455,.T.);
#4660=ORIENTED_EDGE('',*,*,#3456,.F.);
#4661=ORIENTED_EDGE('',*,*,#3457,.F.);
#4662=ORIENTED_EDGE('',*,*,#3458,.F.);
#4663=ORIENTED_EDGE('',*,*,#3455,.F.);
#4664=ORIENTED_EDGE('',*,*,#3459,.T.);
#4665=ORIENTED_EDGE('',*,*,#3457,.T.);
#4666=ORIENTED_EDGE('',*,*,#3459,.F.);
#4667=ORIENTED_EDGE('',*,*,#3458,.T.);
#4668=ORIENTED_EDGE('',*,*,#3460,.T.);
#4669=ORIENTED_EDGE('',*,*,#3461,.T.);
#4670=ORIENTED_EDGE('',*,*,#3460,.F.);
#4671=ORIENTED_EDGE('',*,*,#3462,.F.);
#4672=ORIENTED_EDGE('',*,*,#3463,.T.);
#4673=ORIENTED_EDGE('',*,*,#3456,.T.);
#4674=ORIENTED_EDGE('',*,*,#3463,.F.);
#4675=ORIENTED_EDGE('',*,*,#3462,.T.);
#4676=ORIENTED_EDGE('',*,*,#3461,.F.);
#4677=ORIENTED_EDGE('',*,*,#3464,.F.);
#4678=ORIENTED_EDGE('',*,*,#3465,.T.);
#4679=ORIENTED_EDGE('',*,*,#3466,.F.);
#4680=ORIENTED_EDGE('',*,*,#3465,.F.);
#4681=ORIENTED_EDGE('',*,*,#3467,.F.);
#4682=ORIENTED_EDGE('',*,*,#3468,.F.);
#4683=ORIENTED_EDGE('',*,*,#3469,.F.);
#4684=ORIENTED_EDGE('',*,*,#3470,.T.);
#4685=ORIENTED_EDGE('',*,*,#3471,.T.);
#4686=ORIENTED_EDGE('',*,*,#3472,.F.);
#4687=ORIENTED_EDGE('',*,*,#3473,.T.);
#4688=ORIENTED_EDGE('',*,*,#3470,.F.);
#4689=ORIENTED_EDGE('',*,*,#3464,.T.);
#4690=ORIENTED_EDGE('',*,*,#3469,.T.);
#4691=ORIENTED_EDGE('',*,*,#3474,.F.);
#4692=ORIENTED_EDGE('',*,*,#3475,.F.);
#4693=ORIENTED_EDGE('',*,*,#3471,.F.);
#4694=ORIENTED_EDGE('',*,*,#3467,.T.);
#4695=ORIENTED_EDGE('',*,*,#3473,.F.);
#4696=ORIENTED_EDGE('',*,*,#3476,.F.);
#4697=ORIENTED_EDGE('',*,*,#3477,.F.);
#4698=ORIENTED_EDGE('',*,*,#3476,.T.);
#4699=ORIENTED_EDGE('',*,*,#3472,.T.);
#4700=ORIENTED_EDGE('',*,*,#3475,.T.);
#4701=ORIENTED_EDGE('',*,*,#3478,.F.);
#4702=ORIENTED_EDGE('',*,*,#3477,.T.);
#4703=ORIENTED_EDGE('',*,*,#3478,.T.);
#4704=ORIENTED_EDGE('',*,*,#3474,.T.);
#4705=ORIENTED_EDGE('',*,*,#3468,.T.);
#4706=ORIENTED_EDGE('',*,*,#3466,.T.);
#4707=ORIENTED_EDGE('',*,*,#3479,.F.);
#4708=ORIENTED_EDGE('',*,*,#3480,.T.);
#4709=ORIENTED_EDGE('',*,*,#3481,.T.);
#4710=ORIENTED_EDGE('',*,*,#3480,.F.);
#4711=ORIENTED_EDGE('',*,*,#3482,.F.);
#4712=ORIENTED_EDGE('',*,*,#3483,.T.);
#4713=ORIENTED_EDGE('',*,*,#3484,.T.);
#4714=ORIENTED_EDGE('',*,*,#3483,.F.);
#4715=ORIENTED_EDGE('',*,*,#3482,.T.);
#4716=ORIENTED_EDGE('',*,*,#3479,.T.);
#4717=ORIENTED_EDGE('',*,*,#3484,.F.);
#4718=ORIENTED_EDGE('',*,*,#3481,.F.);
#4719=ORIENTED_EDGE('',*,*,#3485,.F.);
#4720=ORIENTED_EDGE('',*,*,#3486,.T.);
#4721=ORIENTED_EDGE('',*,*,#3487,.T.);
#4722=ORIENTED_EDGE('',*,*,#3486,.F.);
#4723=ORIENTED_EDGE('',*,*,#3488,.F.);
#4724=ORIENTED_EDGE('',*,*,#3489,.T.);
#4725=ORIENTED_EDGE('',*,*,#3490,.T.);
#4726=ORIENTED_EDGE('',*,*,#3489,.F.);
#4727=ORIENTED_EDGE('',*,*,#3488,.T.);
#4728=ORIENTED_EDGE('',*,*,#3485,.T.);
#4729=ORIENTED_EDGE('',*,*,#3490,.F.);
#4730=ORIENTED_EDGE('',*,*,#3487,.F.);
#4731=ORIENTED_EDGE('',*,*,#3491,.F.);
#4732=ORIENTED_EDGE('',*,*,#3492,.T.);
#4733=ORIENTED_EDGE('',*,*,#3493,.T.);
#4734=ORIENTED_EDGE('',*,*,#3492,.F.);
#4735=ORIENTED_EDGE('',*,*,#3494,.F.);
#4736=ORIENTED_EDGE('',*,*,#3495,.T.);
#4737=ORIENTED_EDGE('',*,*,#3496,.T.);
#4738=ORIENTED_EDGE('',*,*,#3495,.F.);
#4739=ORIENTED_EDGE('',*,*,#3494,.T.);
#4740=ORIENTED_EDGE('',*,*,#3491,.T.);
#4741=ORIENTED_EDGE('',*,*,#3496,.F.);
#4742=ORIENTED_EDGE('',*,*,#3493,.F.);
#4743=ORIENTED_EDGE('',*,*,#3497,.T.);
#4744=ORIENTED_EDGE('',*,*,#3498,.T.);
#4745=ORIENTED_EDGE('',*,*,#3499,.T.);
#4746=ORIENTED_EDGE('',*,*,#3500,.F.);
#4747=ORIENTED_EDGE('',*,*,#3501,.T.);
#4748=ORIENTED_EDGE('',*,*,#3502,.T.);
#4749=ORIENTED_EDGE('',*,*,#3503,.T.);
#4750=ORIENTED_EDGE('',*,*,#3498,.F.);
#4751=ORIENTED_EDGE('',*,*,#3504,.T.);
#4752=ORIENTED_EDGE('',*,*,#3505,.T.);
#4753=ORIENTED_EDGE('',*,*,#3506,.T.);
#4754=ORIENTED_EDGE('',*,*,#3502,.F.);
#4755=ORIENTED_EDGE('',*,*,#3507,.T.);
#4756=ORIENTED_EDGE('',*,*,#3508,.T.);
#4757=ORIENTED_EDGE('',*,*,#3509,.T.);
#4758=ORIENTED_EDGE('',*,*,#3505,.F.);
#4759=ORIENTED_EDGE('',*,*,#3510,.T.);
#4760=ORIENTED_EDGE('',*,*,#3511,.T.);
#4761=ORIENTED_EDGE('',*,*,#3512,.T.);
#4762=ORIENTED_EDGE('',*,*,#3508,.F.);
#4763=ORIENTED_EDGE('',*,*,#3513,.T.);
#4764=ORIENTED_EDGE('',*,*,#3500,.T.);
#4765=ORIENTED_EDGE('',*,*,#3514,.T.);
#4766=ORIENTED_EDGE('',*,*,#3511,.F.);
#4767=ORIENTED_EDGE('',*,*,#3513,.F.);
#4768=ORIENTED_EDGE('',*,*,#3510,.F.);
#4769=ORIENTED_EDGE('',*,*,#3507,.F.);
#4770=ORIENTED_EDGE('',*,*,#3504,.F.);
#4771=ORIENTED_EDGE('',*,*,#3501,.F.);
#4772=ORIENTED_EDGE('',*,*,#3497,.F.);
#4773=ORIENTED_EDGE('',*,*,#3514,.F.);
#4774=ORIENTED_EDGE('',*,*,#3499,.F.);
#4775=ORIENTED_EDGE('',*,*,#3503,.F.);
#4776=ORIENTED_EDGE('',*,*,#3506,.F.);
#4777=ORIENTED_EDGE('',*,*,#3509,.F.);
#4778=ORIENTED_EDGE('',*,*,#3512,.F.);
#4779=ORIENTED_EDGE('',*,*,#3515,.F.);
#4780=ORIENTED_EDGE('',*,*,#3516,.F.);
#4781=ORIENTED_EDGE('',*,*,#3517,.F.);
#4782=ORIENTED_EDGE('',*,*,#3518,.T.);
#4783=ORIENTED_EDGE('',*,*,#3516,.T.);
#4784=ORIENTED_EDGE('',*,*,#3518,.F.);
#4785=ORIENTED_EDGE('',*,*,#3519,.F.);
#4786=ORIENTED_EDGE('',*,*,#3520,.T.);
#4787=ORIENTED_EDGE('',*,*,#3517,.T.);
#4788=ORIENTED_EDGE('',*,*,#3520,.F.);
#4789=ORIENTED_EDGE('',*,*,#3521,.F.);
#4790=ORIENTED_EDGE('',*,*,#3522,.T.);
#4791=ORIENTED_EDGE('',*,*,#3519,.T.);
#4792=ORIENTED_EDGE('',*,*,#3522,.F.);
#4793=ORIENTED_EDGE('',*,*,#3521,.T.);
#4794=ORIENTED_EDGE('',*,*,#3523,.F.);
#4795=ORIENTED_EDGE('',*,*,#3524,.F.);
#4796=ORIENTED_EDGE('',*,*,#3525,.T.);
#4797=ORIENTED_EDGE('',*,*,#3523,.T.);
#4798=ORIENTED_EDGE('',*,*,#3525,.F.);
#4799=ORIENTED_EDGE('',*,*,#3515,.T.);
#4800=ORIENTED_EDGE('',*,*,#3526,.T.);
#4801=ORIENTED_EDGE('',*,*,#3524,.T.);
#4802=ORIENTED_EDGE('',*,*,#3526,.F.);
#4803=ORIENTED_EDGE('',*,*,#3527,.F.);
#4804=ORIENTED_EDGE('',*,*,#3528,.T.);
#4805=ORIENTED_EDGE('',*,*,#3529,.F.);
#4806=ORIENTED_EDGE('',*,*,#3528,.F.);
#4807=ORIENTED_EDGE('',*,*,#3530,.F.);
#4808=ORIENTED_EDGE('',*,*,#3531,.T.);
#4809=ORIENTED_EDGE('',*,*,#3532,.F.);
#4810=ORIENTED_EDGE('',*,*,#3531,.F.);
#4811=ORIENTED_EDGE('',*,*,#3533,.F.);
#4812=ORIENTED_EDGE('',*,*,#3534,.T.);
#4813=ORIENTED_EDGE('',*,*,#3535,.F.);
#4814=ORIENTED_EDGE('',*,*,#3534,.F.);
#4815=ORIENTED_EDGE('',*,*,#3536,.F.);
#4816=ORIENTED_EDGE('',*,*,#3537,.T.);
#4817=ORIENTED_EDGE('',*,*,#3538,.F.);
#4818=ORIENTED_EDGE('',*,*,#3537,.F.);
#4819=ORIENTED_EDGE('',*,*,#3539,.F.);
#4820=ORIENTED_EDGE('',*,*,#3540,.F.);
#4821=ORIENTED_EDGE('',*,*,#3541,.F.);
#4822=ORIENTED_EDGE('',*,*,#3542,.F.);
#4823=ORIENTED_EDGE('',*,*,#3543,.F.);
#4824=ORIENTED_EDGE('',*,*,#3544,.F.);
#4825=ORIENTED_EDGE('',*,*,#3545,.F.);
#4826=ORIENTED_EDGE('',*,*,#3546,.F.);
#4827=ORIENTED_EDGE('',*,*,#3547,.F.);
#4828=ORIENTED_EDGE('',*,*,#3548,.F.);
#4829=ORIENTED_EDGE('',*,*,#3549,.F.);
#4830=ORIENTED_EDGE('',*,*,#3550,.F.);
#4831=ORIENTED_EDGE('',*,*,#3551,.F.);
#4832=ORIENTED_EDGE('',*,*,#3552,.F.);
#4833=ORIENTED_EDGE('',*,*,#3553,.F.);
#4834=ORIENTED_EDGE('',*,*,#3554,.F.);
#4835=ORIENTED_EDGE('',*,*,#3540,.T.);
#4836=ORIENTED_EDGE('',*,*,#3555,.T.);
#4837=ORIENTED_EDGE('',*,*,#3556,.T.);
#4838=ORIENTED_EDGE('',*,*,#3557,.F.);
#4839=ORIENTED_EDGE('',*,*,#3544,.T.);
#4840=ORIENTED_EDGE('',*,*,#3558,.T.);
#4841=ORIENTED_EDGE('',*,*,#3559,.T.);
#4842=ORIENTED_EDGE('',*,*,#3560,.F.);
#4843=ORIENTED_EDGE('',*,*,#3548,.T.);
#4844=ORIENTED_EDGE('',*,*,#3561,.T.);
#4845=ORIENTED_EDGE('',*,*,#3562,.T.);
#4846=ORIENTED_EDGE('',*,*,#3563,.F.);
#4847=ORIENTED_EDGE('',*,*,#3541,.T.);
#4848=ORIENTED_EDGE('',*,*,#3557,.T.);
#4849=ORIENTED_EDGE('',*,*,#3564,.T.);
#4850=ORIENTED_EDGE('',*,*,#3565,.T.);
#4851=ORIENTED_EDGE('',*,*,#3566,.T.);
#4852=ORIENTED_EDGE('',*,*,#3567,.T.);
#4853=ORIENTED_EDGE('',*,*,#3568,.T.);
#4854=ORIENTED_EDGE('',*,*,#3569,.T.);
#4855=ORIENTED_EDGE('',*,*,#3570,.T.);
#4856=ORIENTED_EDGE('',*,*,#3571,.T.);
#4857=ORIENTED_EDGE('',*,*,#3552,.T.);
#4858=ORIENTED_EDGE('',*,*,#3572,.T.);
#4859=ORIENTED_EDGE('',*,*,#3573,.T.);
#4860=ORIENTED_EDGE('',*,*,#3574,.T.);
#4861=ORIENTED_EDGE('',*,*,#3575,.T.);
#4862=ORIENTED_EDGE('',*,*,#3576,.T.);
#4863=ORIENTED_EDGE('',*,*,#3577,.T.);
#4864=ORIENTED_EDGE('',*,*,#3578,.T.);
#4865=ORIENTED_EDGE('',*,*,#3579,.T.);
#4866=ORIENTED_EDGE('',*,*,#3580,.T.);
#4867=ORIENTED_EDGE('',*,*,#3549,.T.);
#4868=ORIENTED_EDGE('',*,*,#3563,.T.);
#4869=ORIENTED_EDGE('',*,*,#3581,.T.);
#4870=ORIENTED_EDGE('',*,*,#3582,.T.);
#4871=ORIENTED_EDGE('',*,*,#3583,.T.);
#4872=ORIENTED_EDGE('',*,*,#3584,.T.);
#4873=ORIENTED_EDGE('',*,*,#3585,.T.);
#4874=ORIENTED_EDGE('',*,*,#3586,.T.);
#4875=ORIENTED_EDGE('',*,*,#3587,.T.);
#4876=ORIENTED_EDGE('',*,*,#3588,.T.);
#4877=ORIENTED_EDGE('',*,*,#3545,.T.);
#4878=ORIENTED_EDGE('',*,*,#3560,.T.);
#4879=ORIENTED_EDGE('',*,*,#3589,.T.);
#4880=ORIENTED_EDGE('',*,*,#3590,.T.);
#4881=ORIENTED_EDGE('',*,*,#3591,.T.);
#4882=ORIENTED_EDGE('',*,*,#3592,.T.);
#4883=ORIENTED_EDGE('',*,*,#3593,.T.);
#4884=ORIENTED_EDGE('',*,*,#3594,.T.);
#4885=ORIENTED_EDGE('',*,*,#3595,.T.);
#4886=ORIENTED_EDGE('',*,*,#3596,.T.);
#4887=ORIENTED_EDGE('',*,*,#3529,.T.);
#4888=ORIENTED_EDGE('',*,*,#3532,.T.);
#4889=ORIENTED_EDGE('',*,*,#3535,.T.);
#4890=ORIENTED_EDGE('',*,*,#3538,.T.);
#4891=ORIENTED_EDGE('',*,*,#3551,.T.);
#4892=ORIENTED_EDGE('',*,*,#3597,.T.);
#4893=ORIENTED_EDGE('',*,*,#3598,.T.);
#4894=ORIENTED_EDGE('',*,*,#3572,.F.);
#4895=ORIENTED_EDGE('',*,*,#3553,.T.);
#4896=ORIENTED_EDGE('',*,*,#3571,.F.);
#4897=ORIENTED_EDGE('',*,*,#3599,.T.);
#4898=ORIENTED_EDGE('',*,*,#3600,.T.);
#4899=ORIENTED_EDGE('',*,*,#3570,.F.);
#4900=ORIENTED_EDGE('',*,*,#3601,.F.);
#4901=ORIENTED_EDGE('',*,*,#3602,.F.);
#4902=ORIENTED_EDGE('',*,*,#3599,.F.);
#4903=ORIENTED_EDGE('',*,*,#3569,.F.);
#4904=ORIENTED_EDGE('',*,*,#3603,.F.);
#4905=ORIENTED_EDGE('',*,*,#3604,.F.);
#4906=ORIENTED_EDGE('',*,*,#3601,.T.);
#4907=ORIENTED_EDGE('',*,*,#3565,.F.);
#4908=ORIENTED_EDGE('',*,*,#3605,.F.);
#4909=ORIENTED_EDGE('',*,*,#3606,.F.);
#4910=ORIENTED_EDGE('',*,*,#3607,.F.);
#4911=ORIENTED_EDGE('',*,*,#3564,.F.);
#4912=ORIENTED_EDGE('',*,*,#3556,.F.);
#4913=ORIENTED_EDGE('',*,*,#3608,.F.);
#4914=ORIENTED_EDGE('',*,*,#3605,.T.);
#4915=ORIENTED_EDGE('',*,*,#3607,.T.);
#4916=ORIENTED_EDGE('',*,*,#3609,.F.);
#4917=ORIENTED_EDGE('',*,*,#3610,.T.);
#4918=ORIENTED_EDGE('',*,*,#3566,.F.);
#4919=ORIENTED_EDGE('',*,*,#3539,.T.);
#4920=ORIENTED_EDGE('',*,*,#3611,.F.);
#4921=ORIENTED_EDGE('',*,*,#3612,.T.);
#4922=ORIENTED_EDGE('',*,*,#3613,.T.);
#4923=ORIENTED_EDGE('',*,*,#3614,.T.);
#4924=ORIENTED_EDGE('',*,*,#3615,.T.);
#4925=ORIENTED_EDGE('',*,*,#3616,.T.);
#4926=ORIENTED_EDGE('',*,*,#3617,.T.);
#4927=ORIENTED_EDGE('',*,*,#3609,.T.);
#4928=ORIENTED_EDGE('',*,*,#3606,.T.);
#4929=ORIENTED_EDGE('',*,*,#3608,.T.);
#4930=ORIENTED_EDGE('',*,*,#3555,.F.);
#4931=ORIENTED_EDGE('',*,*,#3527,.T.);
#4932=ORIENTED_EDGE('',*,*,#3554,.T.);
#4933=ORIENTED_EDGE('',*,*,#3600,.F.);
#4934=ORIENTED_EDGE('',*,*,#3602,.T.);
#4935=ORIENTED_EDGE('',*,*,#3604,.T.);
#4936=ORIENTED_EDGE('',*,*,#3618,.T.);
#4937=ORIENTED_EDGE('',*,*,#3619,.T.);
#4938=ORIENTED_EDGE('',*,*,#3620,.T.);
#4939=ORIENTED_EDGE('',*,*,#3621,.T.);
#4940=ORIENTED_EDGE('',*,*,#3622,.T.);
#4941=ORIENTED_EDGE('',*,*,#3623,.T.);
#4942=ORIENTED_EDGE('',*,*,#3624,.T.);
#4943=ORIENTED_EDGE('',*,*,#3597,.F.);
#4944=ORIENTED_EDGE('',*,*,#3536,.T.);
#4945=ORIENTED_EDGE('',*,*,#3625,.F.);
#4946=ORIENTED_EDGE('',*,*,#3626,.T.);
#4947=ORIENTED_EDGE('',*,*,#3627,.F.);
#4948=ORIENTED_EDGE('',*,*,#3619,.F.);
#4949=ORIENTED_EDGE('',*,*,#3628,.T.);
#4950=ORIENTED_EDGE('',*,*,#3567,.F.);
#4951=ORIENTED_EDGE('',*,*,#3610,.F.);
#4952=ORIENTED_EDGE('',*,*,#3617,.F.);
#4953=ORIENTED_EDGE('',*,*,#3629,.F.);
#4954=ORIENTED_EDGE('',*,*,#3626,.F.);
#4955=ORIENTED_EDGE('',*,*,#3627,.T.);
#4956=ORIENTED_EDGE('',*,*,#3625,.T.);
#4957=ORIENTED_EDGE('',*,*,#3629,.T.);
#4958=ORIENTED_EDGE('',*,*,#3616,.F.);
#4959=ORIENTED_EDGE('',*,*,#3630,.T.);
#4960=ORIENTED_EDGE('',*,*,#3631,.T.);
#4961=ORIENTED_EDGE('',*,*,#3632,.T.);
#4962=ORIENTED_EDGE('',*,*,#3633,.T.);
#4963=ORIENTED_EDGE('',*,*,#3632,.F.);
#4964=ORIENTED_EDGE('',*,*,#3634,.T.);
#4965=ORIENTED_EDGE('',*,*,#3635,.T.);
#4966=ORIENTED_EDGE('',*,*,#3636,.F.);
#4967=ORIENTED_EDGE('',*,*,#3637,.T.);
#4968=ORIENTED_EDGE('',*,*,#3638,.T.);
#4969=ORIENTED_EDGE('',*,*,#3639,.T.);
#4970=ORIENTED_EDGE('',*,*,#3640,.F.);
#4971=ORIENTED_EDGE('',*,*,#3641,.T.);
#4972=ORIENTED_EDGE('',*,*,#3642,.T.);
#4973=ORIENTED_EDGE('',*,*,#3643,.T.);
#4974=ORIENTED_EDGE('',*,*,#3620,.F.);
#4975=ORIENTED_EDGE('',*,*,#3603,.T.);
#4976=ORIENTED_EDGE('',*,*,#3568,.F.);
#4977=ORIENTED_EDGE('',*,*,#3628,.F.);
#4978=ORIENTED_EDGE('',*,*,#3618,.F.);
#4979=ORIENTED_EDGE('',*,*,#3542,.T.);
#4980=ORIENTED_EDGE('',*,*,#3596,.F.);
#4981=ORIENTED_EDGE('',*,*,#3644,.T.);
#4982=ORIENTED_EDGE('',*,*,#3611,.T.);
#4983=ORIENTED_EDGE('',*,*,#3595,.F.);
#4984=ORIENTED_EDGE('',*,*,#3645,.F.);
#4985=ORIENTED_EDGE('',*,*,#3612,.F.);
#4986=ORIENTED_EDGE('',*,*,#3644,.F.);
#4987=ORIENTED_EDGE('',*,*,#3594,.F.);
#4988=ORIENTED_EDGE('',*,*,#3646,.F.);
#4989=ORIENTED_EDGE('',*,*,#3613,.F.);
#4990=ORIENTED_EDGE('',*,*,#3645,.T.);
#4991=ORIENTED_EDGE('',*,*,#3590,.F.);
#4992=ORIENTED_EDGE('',*,*,#3647,.F.);
#4993=ORIENTED_EDGE('',*,*,#3648,.F.);
#4994=ORIENTED_EDGE('',*,*,#3649,.F.);
#4995=ORIENTED_EDGE('',*,*,#3589,.F.);
#4996=ORIENTED_EDGE('',*,*,#3559,.F.);
#4997=ORIENTED_EDGE('',*,*,#3650,.F.);
#4998=ORIENTED_EDGE('',*,*,#3647,.T.);
#4999=ORIENTED_EDGE('',*,*,#3649,.T.);
#5000=ORIENTED_EDGE('',*,*,#3651,.F.);
#5001=ORIENTED_EDGE('',*,*,#3652,.T.);
#5002=ORIENTED_EDGE('',*,*,#3591,.F.);
#5003=ORIENTED_EDGE('',*,*,#3543,.T.);
#5004=ORIENTED_EDGE('',*,*,#3653,.F.);
#5005=ORIENTED_EDGE('',*,*,#3654,.T.);
#5006=ORIENTED_EDGE('',*,*,#3655,.T.);
#5007=ORIENTED_EDGE('',*,*,#3656,.T.);
#5008=ORIENTED_EDGE('',*,*,#3657,.T.);
#5009=ORIENTED_EDGE('',*,*,#3636,.T.);
#5010=ORIENTED_EDGE('',*,*,#3658,.T.);
#5011=ORIENTED_EDGE('',*,*,#3651,.T.);
#5012=ORIENTED_EDGE('',*,*,#3648,.T.);
#5013=ORIENTED_EDGE('',*,*,#3650,.T.);
#5014=ORIENTED_EDGE('',*,*,#3558,.F.);
#5015=ORIENTED_EDGE('',*,*,#3530,.T.);
#5016=ORIENTED_EDGE('',*,*,#3631,.F.);
#5017=ORIENTED_EDGE('',*,*,#3659,.T.);
#5018=ORIENTED_EDGE('',*,*,#3634,.F.);
#5019=ORIENTED_EDGE('',*,*,#3630,.F.);
#5020=ORIENTED_EDGE('',*,*,#3615,.F.);
#5021=ORIENTED_EDGE('',*,*,#3660,.T.);
#5022=ORIENTED_EDGE('',*,*,#3592,.F.);
#5023=ORIENTED_EDGE('',*,*,#3652,.F.);
#5024=ORIENTED_EDGE('',*,*,#3658,.F.);
#5025=ORIENTED_EDGE('',*,*,#3635,.F.);
#5026=ORIENTED_EDGE('',*,*,#3659,.F.);
#5027=ORIENTED_EDGE('',*,*,#3646,.T.);
#5028=ORIENTED_EDGE('',*,*,#3593,.F.);
#5029=ORIENTED_EDGE('',*,*,#3660,.F.);
#5030=ORIENTED_EDGE('',*,*,#3614,.F.);
#5031=ORIENTED_EDGE('',*,*,#3546,.T.);
#5032=ORIENTED_EDGE('',*,*,#3588,.F.);
#5033=ORIENTED_EDGE('',*,*,#3661,.T.);
#5034=ORIENTED_EDGE('',*,*,#3653,.T.);
#5035=ORIENTED_EDGE('',*,*,#3587,.F.);
#5036=ORIENTED_EDGE('',*,*,#3662,.F.);
#5037=ORIENTED_EDGE('',*,*,#3654,.F.);
#5038=ORIENTED_EDGE('',*,*,#3661,.F.);
#5039=ORIENTED_EDGE('',*,*,#3586,.F.);
#5040=ORIENTED_EDGE('',*,*,#3663,.F.);
#5041=ORIENTED_EDGE('',*,*,#3655,.F.);
#5042=ORIENTED_EDGE('',*,*,#3662,.T.);
#5043=ORIENTED_EDGE('',*,*,#3582,.F.);
#5044=ORIENTED_EDGE('',*,*,#3664,.F.);
#5045=ORIENTED_EDGE('',*,*,#3665,.F.);
#5046=ORIENTED_EDGE('',*,*,#3666,.F.);
#5047=ORIENTED_EDGE('',*,*,#3581,.F.);
#5048=ORIENTED_EDGE('',*,*,#3562,.F.);
#5049=ORIENTED_EDGE('',*,*,#3667,.F.);
#5050=ORIENTED_EDGE('',*,*,#3664,.T.);
#5051=ORIENTED_EDGE('',*,*,#3666,.T.);
#5052=ORIENTED_EDGE('',*,*,#3668,.F.);
#5053=ORIENTED_EDGE('',*,*,#3669,.T.);
#5054=ORIENTED_EDGE('',*,*,#3583,.F.);
#5055=ORIENTED_EDGE('',*,*,#3547,.T.);
#5056=ORIENTED_EDGE('',*,*,#3670,.F.);
#5057=ORIENTED_EDGE('',*,*,#3671,.T.);
#5058=ORIENTED_EDGE('',*,*,#3672,.T.);
#5059=ORIENTED_EDGE('',*,*,#3673,.T.);
#5060=ORIENTED_EDGE('',*,*,#3674,.T.);
#5061=ORIENTED_EDGE('',*,*,#3640,.T.);
#5062=ORIENTED_EDGE('',*,*,#3675,.T.);
#5063=ORIENTED_EDGE('',*,*,#3668,.T.);
#5064=ORIENTED_EDGE('',*,*,#3665,.T.);
#5065=ORIENTED_EDGE('',*,*,#3667,.T.);
#5066=ORIENTED_EDGE('',*,*,#3561,.F.);
#5067=ORIENTED_EDGE('',*,*,#3533,.T.);
#5068=ORIENTED_EDGE('',*,*,#3638,.F.);
#5069=ORIENTED_EDGE('',*,*,#3676,.T.);
#5070=ORIENTED_EDGE('',*,*,#3637,.F.);
#5071=ORIENTED_EDGE('',*,*,#3657,.F.);
#5072=ORIENTED_EDGE('',*,*,#3677,.T.);
#5073=ORIENTED_EDGE('',*,*,#3584,.F.);
#5074=ORIENTED_EDGE('',*,*,#3669,.F.);
#5075=ORIENTED_EDGE('',*,*,#3675,.F.);
#5076=ORIENTED_EDGE('',*,*,#3639,.F.);
#5077=ORIENTED_EDGE('',*,*,#3676,.F.);
#5078=ORIENTED_EDGE('',*,*,#3663,.T.);
#5079=ORIENTED_EDGE('',*,*,#3585,.F.);
#5080=ORIENTED_EDGE('',*,*,#3677,.F.);
#5081=ORIENTED_EDGE('',*,*,#3656,.F.);
#5082=ORIENTED_EDGE('',*,*,#3550,.T.);
#5083=ORIENTED_EDGE('',*,*,#3580,.F.);
#5084=ORIENTED_EDGE('',*,*,#3678,.T.);
#5085=ORIENTED_EDGE('',*,*,#3670,.T.);
#5086=ORIENTED_EDGE('',*,*,#3579,.F.);
#5087=ORIENTED_EDGE('',*,*,#3679,.F.);
#5088=ORIENTED_EDGE('',*,*,#3671,.F.);
#5089=ORIENTED_EDGE('',*,*,#3678,.F.);
#5090=ORIENTED_EDGE('',*,*,#3624,.F.);
#5091=ORIENTED_EDGE('',*,*,#3680,.T.);
#5092=ORIENTED_EDGE('',*,*,#3573,.F.);
#5093=ORIENTED_EDGE('',*,*,#3598,.F.);
#5094=ORIENTED_EDGE('',*,*,#3623,.F.);
#5095=ORIENTED_EDGE('',*,*,#3681,.F.);
#5096=ORIENTED_EDGE('',*,*,#3574,.F.);
#5097=ORIENTED_EDGE('',*,*,#3680,.F.);
#5098=ORIENTED_EDGE('',*,*,#3578,.F.);
#5099=ORIENTED_EDGE('',*,*,#3682,.F.);
#5100=ORIENTED_EDGE('',*,*,#3672,.F.);
#5101=ORIENTED_EDGE('',*,*,#3679,.T.);
#5102=ORIENTED_EDGE('',*,*,#3642,.F.);
#5103=ORIENTED_EDGE('',*,*,#3683,.T.);
#5104=ORIENTED_EDGE('',*,*,#3641,.F.);
#5105=ORIENTED_EDGE('',*,*,#3674,.F.);
#5106=ORIENTED_EDGE('',*,*,#3684,.T.);
#5107=ORIENTED_EDGE('',*,*,#3576,.F.);
#5108=ORIENTED_EDGE('',*,*,#3685,.F.);
#5109=ORIENTED_EDGE('',*,*,#3621,.F.);
#5110=ORIENTED_EDGE('',*,*,#3643,.F.);
#5111=ORIENTED_EDGE('',*,*,#3683,.F.);
#5112=ORIENTED_EDGE('',*,*,#3682,.T.);
#5113=ORIENTED_EDGE('',*,*,#3577,.F.);
#5114=ORIENTED_EDGE('',*,*,#3684,.F.);
#5115=ORIENTED_EDGE('',*,*,#3673,.F.);
#5116=ORIENTED_EDGE('',*,*,#3681,.T.);
#5117=ORIENTED_EDGE('',*,*,#3622,.F.);
#5118=ORIENTED_EDGE('',*,*,#3685,.T.);
#5119=ORIENTED_EDGE('',*,*,#3575,.F.);
#5120=ORIENTED_EDGE('',*,*,#3633,.F.);
#5121=ORIENTED_EDGE('',*,*,#3686,.F.);
#5122=ORIENTED_EDGE('',*,*,#3686,.T.);
#5123=ORIENTED_EDGE('',*,*,#3687,.T.);
#5124=ORIENTED_EDGE('',*,*,#3688,.T.);
#5125=ORIENTED_EDGE('',*,*,#3687,.F.);
#5126=ORIENTED_EDGE('',*,*,#3688,.F.);
#5127=ORIENTED_EDGE('',*,*,#3689,.F.);
#5128=ORIENTED_EDGE('',*,*,#3690,.T.);
#5129=ORIENTED_EDGE('',*,*,#3691,.T.);
#5130=ORIENTED_EDGE('',*,*,#3690,.F.);
#5131=ORIENTED_EDGE('',*,*,#3692,.F.);
#5132=ORIENTED_EDGE('',*,*,#3693,.T.);
#5133=ORIENTED_EDGE('',*,*,#3694,.T.);
#5134=ORIENTED_EDGE('',*,*,#3693,.F.);
#5135=ORIENTED_EDGE('',*,*,#3692,.T.);
#5136=ORIENTED_EDGE('',*,*,#3689,.T.);
#5137=ORIENTED_EDGE('',*,*,#3694,.F.);
#5138=ORIENTED_EDGE('',*,*,#3691,.F.);
#5139=ORIENTED_EDGE('',*,*,#3695,.F.);
#5140=ORIENTED_EDGE('',*,*,#3696,.F.);
#5141=ORIENTED_EDGE('',*,*,#3697,.F.);
#5142=ORIENTED_EDGE('',*,*,#3698,.F.);
#5143=ORIENTED_EDGE('',*,*,#3699,.T.);
#5144=ORIENTED_EDGE('',*,*,#3696,.T.);
#5145=ORIENTED_EDGE('',*,*,#3700,.F.);
#5146=ORIENTED_EDGE('',*,*,#3701,.T.);
#5147=ORIENTED_EDGE('',*,*,#3702,.F.);
#5148=ORIENTED_EDGE('',*,*,#3697,.T.);
#5149=ORIENTED_EDGE('',*,*,#3699,.F.);
#5150=ORIENTED_EDGE('',*,*,#3703,.F.);
#5151=ORIENTED_EDGE('',*,*,#3701,.F.);
#5152=ORIENTED_EDGE('',*,*,#3704,.F.);
#5153=ORIENTED_EDGE('',*,*,#3705,.F.);
#5154=ORIENTED_EDGE('',*,*,#3706,.F.);
#5155=ORIENTED_EDGE('',*,*,#3707,.F.);
#5156=ORIENTED_EDGE('',*,*,#3708,.F.);
#5157=ORIENTED_EDGE('',*,*,#3709,.T.);
#5158=ORIENTED_EDGE('',*,*,#3710,.F.);
#5159=ORIENTED_EDGE('',*,*,#3711,.T.);
#5160=ORIENTED_EDGE('',*,*,#3712,.F.);
#5161=ORIENTED_EDGE('',*,*,#3713,.F.);
#5162=ORIENTED_EDGE('',*,*,#3705,.T.);
#5163=ORIENTED_EDGE('',*,*,#3714,.F.);
#5164=ORIENTED_EDGE('',*,*,#3709,.F.);
#5165=ORIENTED_EDGE('',*,*,#3715,.F.);
#5166=ORIENTED_EDGE('',*,*,#3711,.F.);
#5167=ORIENTED_EDGE('',*,*,#3716,.F.);
#5168=ORIENTED_EDGE('',*,*,#3717,.T.);
#5169=ORIENTED_EDGE('',*,*,#3714,.T.);
#5170=ORIENTED_EDGE('',*,*,#3704,.T.);
#5171=ORIENTED_EDGE('',*,*,#3713,.T.);
#5172=ORIENTED_EDGE('',*,*,#3718,.T.);
#5173=ORIENTED_EDGE('',*,*,#3719,.T.);
#5174=ORIENTED_EDGE('',*,*,#3718,.F.);
#5175=ORIENTED_EDGE('',*,*,#3712,.T.);
#5176=ORIENTED_EDGE('',*,*,#3715,.T.);
#5177=ORIENTED_EDGE('',*,*,#3710,.T.);
#5178=ORIENTED_EDGE('',*,*,#3717,.F.);
#5179=ORIENTED_EDGE('',*,*,#3702,.T.);
#5180=ORIENTED_EDGE('',*,*,#3703,.T.);
#5181=ORIENTED_EDGE('',*,*,#3700,.T.);
#5182=ORIENTED_EDGE('',*,*,#3695,.T.);
#5183=ORIENTED_EDGE('',*,*,#3720,.F.);
#5184=ORIENTED_EDGE('',*,*,#3721,.T.);
#5185=ORIENTED_EDGE('',*,*,#3708,.T.);
#5186=ORIENTED_EDGE('',*,*,#3722,.T.);
#5187=ORIENTED_EDGE('',*,*,#3723,.T.);
#5188=ORIENTED_EDGE('',*,*,#3722,.F.);
#5189=ORIENTED_EDGE('',*,*,#3707,.T.);
#5190=ORIENTED_EDGE('',*,*,#3706,.T.);
#5191=ORIENTED_EDGE('',*,*,#3721,.F.);
#5192=ORIENTED_EDGE('',*,*,#3698,.T.);
#5193=ORIENTED_EDGE('',*,*,#3720,.T.);
#5194=ORIENTED_EDGE('',*,*,#3716,.T.);
#5195=ORIENTED_EDGE('',*,*,#3723,.F.);
#5196=ORIENTED_EDGE('',*,*,#3719,.F.);
#5197=ORIENTED_EDGE('',*,*,#3724,.F.);
#5198=ORIENTED_EDGE('',*,*,#3725,.F.);
#5199=ORIENTED_EDGE('',*,*,#3726,.T.);
#5200=ORIENTED_EDGE('',*,*,#3727,.T.);
#5201=ORIENTED_EDGE('',*,*,#3728,.F.);
#5202=ORIENTED_EDGE('',*,*,#3729,.F.);
#5203=ORIENTED_EDGE('',*,*,#3730,.T.);
#5204=ORIENTED_EDGE('',*,*,#3731,.T.);
#5205=ORIENTED_EDGE('',*,*,#3726,.F.);
#5206=ORIENTED_EDGE('',*,*,#3732,.F.);
#5207=ORIENTED_EDGE('',*,*,#3733,.T.);
#5208=ORIENTED_EDGE('',*,*,#3734,.T.);
#5209=ORIENTED_EDGE('',*,*,#3730,.F.);
#5210=ORIENTED_EDGE('',*,*,#3735,.F.);
#5211=ORIENTED_EDGE('',*,*,#3736,.T.);
#5212=ORIENTED_EDGE('',*,*,#3737,.T.);
#5213=ORIENTED_EDGE('',*,*,#3733,.F.);
#5214=ORIENTED_EDGE('',*,*,#3738,.F.);
#5215=ORIENTED_EDGE('',*,*,#3739,.T.);
#5216=ORIENTED_EDGE('',*,*,#3740,.T.);
#5217=ORIENTED_EDGE('',*,*,#3736,.F.);
#5218=ORIENTED_EDGE('',*,*,#3741,.F.);
#5219=ORIENTED_EDGE('',*,*,#3728,.T.);
#5220=ORIENTED_EDGE('',*,*,#3742,.T.);
#5221=ORIENTED_EDGE('',*,*,#3739,.F.);
#5222=ORIENTED_EDGE('',*,*,#3742,.F.);
#5223=ORIENTED_EDGE('',*,*,#3727,.F.);
#5224=ORIENTED_EDGE('',*,*,#3731,.F.);
#5225=ORIENTED_EDGE('',*,*,#3734,.F.);
#5226=ORIENTED_EDGE('',*,*,#3737,.F.);
#5227=ORIENTED_EDGE('',*,*,#3740,.F.);
#5228=ORIENTED_EDGE('',*,*,#3743,.F.);
#5229=ORIENTED_EDGE('',*,*,#3725,.T.);
#5230=ORIENTED_EDGE('',*,*,#3741,.T.);
#5231=ORIENTED_EDGE('',*,*,#3738,.T.);
#5232=ORIENTED_EDGE('',*,*,#3735,.T.);
#5233=ORIENTED_EDGE('',*,*,#3732,.T.);
#5234=ORIENTED_EDGE('',*,*,#3729,.T.);
#5235=ORIENTED_EDGE('',*,*,#3744,.F.);
#5236=ORIENTED_EDGE('',*,*,#3745,.T.);
#5237=ORIENTED_EDGE('',*,*,#3743,.T.);
#5238=ORIENTED_EDGE('',*,*,#3745,.F.);
#5239=ORIENTED_EDGE('',*,*,#3724,.T.);
#5240=ORIENTED_EDGE('',*,*,#3746,.T.);
#5241=ORIENTED_EDGE('',*,*,#3744,.T.);
#5242=ORIENTED_EDGE('',*,*,#3746,.F.);
#5243=CYLINDRICAL_SURFACE('',#6013,0.21);
#5244=CYLINDRICAL_SURFACE('',#6016,0.21);
#5245=CYLINDRICAL_SURFACE('',#6019,0.21);
#5246=CYLINDRICAL_SURFACE('',#6022,0.21);
#5247=CYLINDRICAL_SURFACE('',#6046,0.25);
#5248=CYLINDRICAL_SURFACE('',#6048,0.165);
#5249=CYLINDRICAL_SURFACE('',#6052,0.165);
#5250=CYLINDRICAL_SURFACE('',#6056,0.165);
#5251=CYLINDRICAL_SURFACE('',#6060,0.165);
#5252=CYLINDRICAL_SURFACE('',#6064,1.5);
#5253=CYLINDRICAL_SURFACE('',#6069,1.02);
#5254=CYLINDRICAL_SURFACE('',#6071,0.25);
#5255=CYLINDRICAL_SURFACE('',#6073,0.165);
#5256=CYLINDRICAL_SURFACE('',#6077,0.165);
#5257=CYLINDRICAL_SURFACE('',#6081,0.165);
#5258=CYLINDRICAL_SURFACE('',#6085,0.165);
#5259=CYLINDRICAL_SURFACE('',#6089,1.5);
#5260=CYLINDRICAL_SURFACE('',#6094,1.02);
#5261=CYLINDRICAL_SURFACE('',#6096,0.5);
#5262=CYLINDRICAL_SURFACE('',#6099,0.5);
#5263=CYLINDRICAL_SURFACE('',#6104,0.5);
#5264=CYLINDRICAL_SURFACE('',#6107,0.5);
#5265=CYLINDRICAL_SURFACE('',#6112,0.5);
#5266=CYLINDRICAL_SURFACE('',#6115,0.5);
#5267=CYLINDRICAL_SURFACE('',#6120,0.5);
#5268=CYLINDRICAL_SURFACE('',#6123,0.5);
#5269=CYLINDRICAL_SURFACE('',#6133,0.275);
#5270=CYLINDRICAL_SURFACE('',#6135,0.275);
#5271=CYLINDRICAL_SURFACE('',#6137,0.275);
#5272=CYLINDRICAL_SURFACE('',#6139,0.275);
#5273=CYLINDRICAL_SURFACE('',#6147,0.375);
#5274=CYLINDRICAL_SURFACE('',#6158,0.375);
#5275=CYLINDRICAL_SURFACE('',#6164,0.375);
#5276=CYLINDRICAL_SURFACE('',#6170,0.375);
#5277=CYLINDRICAL_SURFACE('',#6178,0.225);
#5278=CYLINDRICAL_SURFACE('',#6180,0.225);
#5279=CYLINDRICAL_SURFACE('',#6182,0.225);
#5280=CYLINDRICAL_SURFACE('',#6184,0.225);
#5281=CYLINDRICAL_SURFACE('',#6186,1.49);
#5282=CYLINDRICAL_SURFACE('',#6191,0.71);
#5283=CYLINDRICAL_SURFACE('',#6192,2.);
#5284=CYLINDRICAL_SURFACE('',#6196,0.375);
#5285=CYLINDRICAL_SURFACE('',#6207,0.375);
#5286=CYLINDRICAL_SURFACE('',#6213,0.375);
#5287=CYLINDRICAL_SURFACE('',#6219,0.375);
#5288=CYLINDRICAL_SURFACE('',#6227,0.225);
#5289=CYLINDRICAL_SURFACE('',#6229,0.225);
#5290=CYLINDRICAL_SURFACE('',#6231,0.225);
#5291=CYLINDRICAL_SURFACE('',#6233,0.225);
#5292=CYLINDRICAL_SURFACE('',#6235,1.49);
#5293=CYLINDRICAL_SURFACE('',#6240,0.71);
#5294=CYLINDRICAL_SURFACE('',#6241,2.);
#5295=CYLINDRICAL_SURFACE('',#6249,0.425);
#5296=CYLINDRICAL_SURFACE('',#6257,0.24505);
#5297=CYLINDRICAL_SURFACE('',#6278,0.976185);
#5298=CYLINDRICAL_SURFACE('',#6280,0.5);
#5299=CYLINDRICAL_SURFACE('',#6286,0.976185);
#5300=CYLINDRICAL_SURFACE('',#6298,1.023815);
#5301=CYLINDRICAL_SURFACE('',#6305,1.5);
#5302=CYLINDRICAL_SURFACE('',#6310,1.023815);
#5303=CYLINDRICAL_SURFACE('',#6332,1.019052);
#5304=CYLINDRICAL_SURFACE('',#6372,0.980948);
#5305=CYLINDRICAL_SURFACE('',#6386,1.013815);
#5306=CYLINDRICAL_SURFACE('',#6390,0.991185);
#5307=CYLINDRICAL_SURFACE('',#6394,1.013815);
#5308=CYLINDRICAL_SURFACE('',#6398,0.991185);
#5309=CYLINDRICAL_SURFACE('',#6406,0.165);
#5310=CYLINDRICAL_SURFACE('',#6410,0.25);
#5311=CYLINDRICAL_SURFACE('',#6413,0.5);
#5312=CYLINDRICAL_SURFACE('',#6429,1.);
#5313=CYLINDRICAL_SURFACE('',#6430,1.);
#5314=CYLINDRICAL_SURFACE('',#6434,0.7);
#5315=CYLINDRICAL_SURFACE('',#6435,0.5);
#5316=CYLINDRICAL_SURFACE('',#6437,0.5);
#5317=CYLINDRICAL_SURFACE('',#6442,0.505);
#5318=CYLINDRICAL_SURFACE('',#6445,0.7);
#5319=CYLINDRICAL_SURFACE('',#6454,0.165);
#5320=CYLINDRICAL_SURFACE('',#6459,0.165);
#5321=CYLINDRICAL_SURFACE('',#6462,0.505);
#5322=CYLINDRICAL_SURFACE('',#6465,0.9);
#5323=CYLINDRICAL_SURFACE('',#6477,0.5);
#5324=CYLINDRICAL_SURFACE('',#6478,0.3);
#5325=CYLINDRICAL_SURFACE('',#6480,0.3);
#5326=CYLINDRICAL_SURFACE('',#6485,0.5);
#5327=CYLINDRICAL_SURFACE('',#6488,0.6);
#5328=CYLINDRICAL_SURFACE('',#6495,1.8);
#5329=CYLINDRICAL_SURFACE('',#6499,0.505);
#5330=CYLINDRICAL_SURFACE('',#6502,0.7);
#5331=CYLINDRICAL_SURFACE('',#6508,0.225);
#5332=CYLINDRICAL_SURFACE('',#6511,0.7);
#5333=CYLINDRICAL_SURFACE('',#6517,0.4);
#5334=CYLINDRICAL_SURFACE('',#6520,1.4);
#5335=CYLINDRICAL_SURFACE('',#6540,0.35);
#5336=CYLINDRICAL_SURFACE('',#6548,0.1954);
#5337=CYLINDRICAL_SURFACE('',#6571,0.165);
#5338=CYLINDRICAL_SURFACE('',#6574,0.165);
#5339=CYLINDRICAL_SURFACE('',#6577,0.165);
#5340=CYLINDRICAL_SURFACE('',#6580,0.165);
#5341=CYLINDRICAL_SURFACE('',#6583,1.82);
#5342=CYLINDRICAL_SURFACE('',#6586,1.82);
#5343=CYLINDRICAL_SURFACE('',#6589,1.82);
#5344=CYLINDRICAL_SURFACE('',#6592,1.82);
#5345=CYLINDRICAL_SURFACE('',#6595,3.);
#5346=CYLINDRICAL_SURFACE('',#6598,3.);
#5347=CYLINDRICAL_SURFACE('',#6601,3.);
#5348=CYLINDRICAL_SURFACE('',#6614,3.);
#5349=CYLINDRICAL_SURFACE('',#6616,3.);
#5350=CYLINDRICAL_SURFACE('',#6635,0.32);
#5351=CYLINDRICAL_SURFACE('',#6636,0.7);
#5352=CYLINDRICAL_SURFACE('',#6645,3.);
#5353=CYLINDRICAL_SURFACE('',#6657,0.32);
#5354=CYLINDRICAL_SURFACE('',#6659,3.);
#5355=CYLINDRICAL_SURFACE('',#6671,0.32);
#5356=CYLINDRICAL_SURFACE('',#6673,3.);
#5357=CYLINDRICAL_SURFACE('',#6680,0.32);
#5358=CYLINDRICAL_SURFACE('',#6685,0.5);
#5359=CYLINDRICAL_SURFACE('',#6689,0.505);
#5360=CYLINDRICAL_SURFACE('',#6692,0.7);
#5361=CYLINDRICAL_SURFACE('',#6701,0.165);
#5362=CYLINDRICAL_SURFACE('',#6706,0.165);
#5363=CYLINDRICAL_SURFACE('',#6709,0.505);
#5364=CYLINDRICAL_SURFACE('',#6712,0.9);
#5365=CYLINDRICAL_SURFACE('',#6731,0.1954);
#5366=ADVANCED_FACE('',(#652),#5243,.F.);
#5367=ADVANCED_FACE('',(#653),#5244,.F.);
#5368=ADVANCED_FACE('',(#654),#5245,.F.);
#5369=ADVANCED_FACE('',(#655),#5246,.F.);
#5370=ADVANCED_FACE('',(#656),#472,.T.);
#5371=ADVANCED_FACE('',(#657),#473,.T.);
#5372=ADVANCED_FACE('',(#658),#474,.T.);
#5373=ADVANCED_FACE('',(#659),#475,.T.);
#5374=ADVANCED_FACE('',(#660,#367,#368,#369,#370),#476,.T.);
#5375=ADVANCED_FACE('',(#661,#371,#372,#373,#374),#477,.F.);
#5376=ADVANCED_FACE('',(#662),#478,.T.);
#5377=ADVANCED_FACE('',(#663),#479,.T.);
#5378=ADVANCED_FACE('',(#664),#480,.T.);
#5379=ADVANCED_FACE('',(#665),#481,.T.);
#5380=ADVANCED_FACE('',(#666),#482,.T.);
#5381=ADVANCED_FACE('',(#667),#483,.F.);
#5382=ADVANCED_FACE('',(#668),#484,.T.);
#5383=ADVANCED_FACE('',(#669),#485,.T.);
#5384=ADVANCED_FACE('',(#670),#486,.T.);
#5385=ADVANCED_FACE('',(#671),#487,.T.);
#5386=ADVANCED_FACE('',(#672),#488,.T.);
#5387=ADVANCED_FACE('',(#673),#489,.F.);
#5388=ADVANCED_FACE('',(#674),#5247,.F.);
#5389=ADVANCED_FACE('',(#675),#5248,.F.);
#5390=ADVANCED_FACE('',(#676),#490,.T.);
#5391=ADVANCED_FACE('',(#677),#5249,.F.);
#5392=ADVANCED_FACE('',(#678),#491,.T.);
#5393=ADVANCED_FACE('',(#679),#5250,.F.);
#5394=ADVANCED_FACE('',(#680),#492,.T.);
#5395=ADVANCED_FACE('',(#681),#5251,.F.);
#5396=ADVANCED_FACE('',(#682),#493,.T.);
#5397=ADVANCED_FACE('',(#683),#5252,.F.);
#5398=ADVANCED_FACE('',(#684,#375),#494,.T.);
#5399=ADVANCED_FACE('',(#685,#376),#5253,.F.);
#5400=ADVANCED_FACE('',(#686),#5254,.F.);
#5401=ADVANCED_FACE('',(#687),#5255,.F.);
#5402=ADVANCED_FACE('',(#688),#495,.T.);
#5403=ADVANCED_FACE('',(#689),#5256,.F.);
#5404=ADVANCED_FACE('',(#690),#496,.T.);
#5405=ADVANCED_FACE('',(#691),#5257,.F.);
#5406=ADVANCED_FACE('',(#692),#497,.T.);
#5407=ADVANCED_FACE('',(#693),#5258,.F.);
#5408=ADVANCED_FACE('',(#694),#498,.T.);
#5409=ADVANCED_FACE('',(#695),#5259,.F.);
#5410=ADVANCED_FACE('',(#696,#377),#499,.T.);
#5411=ADVANCED_FACE('',(#697,#378),#5260,.F.);
#5412=ADVANCED_FACE('',(#698),#5261,.F.);
#5413=ADVANCED_FACE('',(#699),#5262,.F.);
#5414=ADVANCED_FACE('',(#700,#379),#500,.T.);
#5415=ADVANCED_FACE('',(#701),#5263,.F.);
#5416=ADVANCED_FACE('',(#702),#5264,.F.);
#5417=ADVANCED_FACE('',(#703,#380),#501,.T.);
#5418=ADVANCED_FACE('',(#704),#5265,.F.);
#5419=ADVANCED_FACE('',(#705),#5266,.F.);
#5420=ADVANCED_FACE('',(#706,#381),#502,.T.);
#5421=ADVANCED_FACE('',(#707),#5267,.F.);
#5422=ADVANCED_FACE('',(#708),#5268,.F.);
#5423=ADVANCED_FACE('',(#709,#382),#503,.T.);
#5424=ADVANCED_FACE('',(#710),#504,.T.);
#5425=ADVANCED_FACE('',(#711),#505,.T.);
#5426=ADVANCED_FACE('',(#712),#506,.T.);
#5427=ADVANCED_FACE('',(#713,#383,#384,#385,#386,#387,#388,#389,#390,#391,
#392),#507,.T.);
#5428=ADVANCED_FACE('',(#714),#508,.T.);
#5429=ADVANCED_FACE('',(#715),#5269,.F.);
#5430=ADVANCED_FACE('',(#716),#5270,.F.);
#5431=ADVANCED_FACE('',(#717),#5271,.F.);
#5432=ADVANCED_FACE('',(#718),#5272,.F.);
#5433=ADVANCED_FACE('',(#719),#509,.T.);
#5434=ADVANCED_FACE('',(#720),#510,.T.);
#5435=ADVANCED_FACE('',(#721,#393,#394),#511,.T.);
#5436=ADVANCED_FACE('',(#722),#512,.T.);
#5437=ADVANCED_FACE('',(#723,#395,#396,#397,#398,#399,#400),#513,.F.);
#5438=ADVANCED_FACE('',(#724),#5273,.F.);
#5439=ADVANCED_FACE('',(#725,#401),#514,.T.);
#5440=ADVANCED_FACE('',(#726,#402),#515,.T.);
#5441=ADVANCED_FACE('',(#727),#5274,.F.);
#5442=ADVANCED_FACE('',(#728,#403),#516,.T.);
#5443=ADVANCED_FACE('',(#729),#5275,.F.);
#5444=ADVANCED_FACE('',(#730,#404),#517,.T.);
#5445=ADVANCED_FACE('',(#731),#5276,.F.);
#5446=ADVANCED_FACE('',(#732,#405),#518,.T.);
#5447=ADVANCED_FACE('',(#733),#5277,.F.);
#5448=ADVANCED_FACE('',(#734),#5278,.F.);
#5449=ADVANCED_FACE('',(#735),#5279,.F.);
#5450=ADVANCED_FACE('',(#736),#5280,.F.);
#5451=ADVANCED_FACE('',(#737),#5281,.T.);
#5452=ADVANCED_FACE('',(#738,#406),#519,.F.);
#5453=ADVANCED_FACE('',(#739),#5282,.F.);
#5454=ADVANCED_FACE('',(#740),#5283,.T.);
#5455=ADVANCED_FACE('',(#741,#407,#408,#409,#410,#411),#520,.F.);
#5456=ADVANCED_FACE('',(#742),#5284,.F.);
#5457=ADVANCED_FACE('',(#743,#412),#521,.T.);
#5458=ADVANCED_FACE('',(#744,#413),#522,.T.);
#5459=ADVANCED_FACE('',(#745),#5285,.F.);
#5460=ADVANCED_FACE('',(#746,#414),#523,.T.);
#5461=ADVANCED_FACE('',(#747),#5286,.F.);
#5462=ADVANCED_FACE('',(#748,#415),#524,.T.);
#5463=ADVANCED_FACE('',(#749),#5287,.F.);
#5464=ADVANCED_FACE('',(#750,#416),#525,.T.);
#5465=ADVANCED_FACE('',(#751),#5288,.F.);
#5466=ADVANCED_FACE('',(#752),#5289,.F.);
#5467=ADVANCED_FACE('',(#753),#5290,.F.);
#5468=ADVANCED_FACE('',(#754),#5291,.F.);
#5469=ADVANCED_FACE('',(#755),#5292,.T.);
#5470=ADVANCED_FACE('',(#756,#417),#526,.F.);
#5471=ADVANCED_FACE('',(#757),#5293,.F.);
#5472=ADVANCED_FACE('',(#758),#5294,.T.);
#5473=ADVANCED_FACE('',(#759,#418,#419,#420,#421,#422),#527,.F.);
#5474=ADVANCED_FACE('',(#760),#528,.T.);
#5475=ADVANCED_FACE('',(#761),#199,.T.);
#5476=ADVANCED_FACE('',(#762),#5295,.T.);
#5477=ADVANCED_FACE('',(#763),#200,.T.);
#5478=ADVANCED_FACE('',(#764,#423),#529,.T.);
#5479=ADVANCED_FACE('',(#765),#201,.T.);
#5480=ADVANCED_FACE('',(#766),#5296,.T.);
#5481=ADVANCED_FACE('',(#767),#202,.T.);
#5482=ADVANCED_FACE('',(#768),#530,.T.);
#5483=ADVANCED_FACE('',(#769),#531,.F.);
#5484=ADVANCED_FACE('',(#770),#532,.F.);
#5485=ADVANCED_FACE('',(#771),#533,.F.);
#5486=ADVANCED_FACE('',(#772),#534,.F.);
#5487=ADVANCED_FACE('',(#773),#535,.F.);
#5488=ADVANCED_FACE('',(#774),#536,.F.);
#5489=ADVANCED_FACE('',(#775),#537,.F.);
#5490=ADVANCED_FACE('',(#776),#538,.F.);
#5491=ADVANCED_FACE('',(#777),#195,.F.);
#5492=ADVANCED_FACE('',(#778),#5297,.T.);
#5493=ADVANCED_FACE('',(#779),#5298,.F.);
#5494=ADVANCED_FACE('',(#780),#203,.F.);
#5495=ADVANCED_FACE('',(#781,#424),#539,.T.);
#5496=ADVANCED_FACE('',(#782),#5299,.T.);
#5497=ADVANCED_FACE('',(#783,#425),#540,.T.);
#5498=ADVANCED_FACE('',(#784),#204,.F.);
#5499=ADVANCED_FACE('',(#785),#196,.F.);
#5500=ADVANCED_FACE('',(#786),#5300,.F.);
#5501=ADVANCED_FACE('',(#787,#426),#541,.T.);
#5502=ADVANCED_FACE('',(#788),#205,.T.);
#5503=ADVANCED_FACE('',(#789),#5301,.T.);
#5504=ADVANCED_FACE('',(#790),#206,.T.);
#5505=ADVANCED_FACE('',(#791,#427),#542,.T.);
#5506=ADVANCED_FACE('',(#792),#5302,.F.);
#5507=ADVANCED_FACE('',(#793),#179,.T.);
#5508=ADVANCED_FACE('',(#794),#180,.T.);
#5509=ADVANCED_FACE('',(#795),#181,.T.);
#5510=ADVANCED_FACE('',(#796),#182,.T.);
#5511=ADVANCED_FACE('',(#797),#183,.T.);
#5512=ADVANCED_FACE('',(#798),#184,.T.);
#5513=ADVANCED_FACE('',(#799),#185,.T.);
#5514=ADVANCED_FACE('',(#800),#186,.T.);
#5515=ADVANCED_FACE('',(#801),#187,.F.);
#5516=ADVANCED_FACE('',(#802),#5303,.T.);
#5517=ADVANCED_FACE('',(#803),#543,.T.);
#5518=ADVANCED_FACE('',(#804),#188,.F.);
#5519=ADVANCED_FACE('',(#805),#544,.T.);
#5520=ADVANCED_FACE('',(#806),#189,.F.);
#5521=ADVANCED_FACE('',(#807),#545,.T.);
#5522=ADVANCED_FACE('',(#808),#190,.F.);
#5523=ADVANCED_FACE('',(#809),#546,.T.);
#5524=ADVANCED_FACE('',(#810),#191,.F.);
#5525=ADVANCED_FACE('',(#811),#547,.T.);
#5526=ADVANCED_FACE('',(#812),#192,.F.);
#5527=ADVANCED_FACE('',(#813),#548,.T.);
#5528=ADVANCED_FACE('',(#814),#193,.F.);
#5529=ADVANCED_FACE('',(#815),#5304,.F.);
#5530=ADVANCED_FACE('',(#816),#549,.T.);
#5531=ADVANCED_FACE('',(#817),#194,.F.);
#5532=ADVANCED_FACE('',(#818,#428),#550,.T.);
#5533=ADVANCED_FACE('',(#819),#551,.T.);
#5534=ADVANCED_FACE('',(#820,#429),#552,.T.);
#5535=ADVANCED_FACE('',(#821),#5305,.T.);
#5536=ADVANCED_FACE('',(#822,#430),#553,.T.);
#5537=ADVANCED_FACE('',(#823),#5306,.F.);
#5538=ADVANCED_FACE('',(#824,#431),#554,.T.);
#5539=ADVANCED_FACE('',(#825),#5307,.T.);
#5540=ADVANCED_FACE('',(#826,#432),#555,.T.);
#5541=ADVANCED_FACE('',(#827),#5308,.F.);
#5542=ADVANCED_FACE('',(#828),#5309,.F.);
#5543=ADVANCED_FACE('',(#829),#556,.T.);
#5544=ADVANCED_FACE('',(#830),#5310,.F.);
#5545=ADVANCED_FACE('',(#831),#5311,.T.);
#5546=ADVANCED_FACE('',(#832,#433,#434),#557,.F.);
#5547=ADVANCED_FACE('',(#833),#558,.T.);
#5548=ADVANCED_FACE('',(#834),#559,.T.);
#5549=ADVANCED_FACE('',(#835),#560,.T.);
#5550=ADVANCED_FACE('',(#836),#561,.T.);
#5551=ADVANCED_FACE('',(#837),#562,.T.);
#5552=ADVANCED_FACE('',(#838,#435,#436),#563,.T.);
#5553=ADVANCED_FACE('',(#839),#5312,.T.);
#5554=ADVANCED_FACE('',(#840),#5313,.T.);
#5555=ADVANCED_FACE('',(#841,#437),#564,.F.);
#5556=ADVANCED_FACE('',(#842),#5314,.T.);
#5557=ADVANCED_FACE('',(#843),#5315,.T.);
#5558=ADVANCED_FACE('',(#844),#5316,.T.);
#5559=ADVANCED_FACE('',(#845,#438),#565,.T.);
#5560=ADVANCED_FACE('',(#846),#566,.F.);
#5561=ADVANCED_FACE('',(#847),#5317,.F.);
#5562=ADVANCED_FACE('',(#848),#5318,.T.);
#5563=ADVANCED_FACE('',(#849,#439),#567,.T.);
#5564=ADVANCED_FACE('',(#850,#440),#568,.F.);
#5565=ADVANCED_FACE('',(#851),#569,.F.);
#5566=ADVANCED_FACE('',(#852),#5319,.F.);
#5567=ADVANCED_FACE('',(#853),#570,.F.);
#5568=ADVANCED_FACE('',(#854),#571,.F.);
#5569=ADVANCED_FACE('',(#855),#5320,.F.);
#5570=ADVANCED_FACE('',(#856),#572,.F.);
#5571=ADVANCED_FACE('',(#857,#441),#5321,.F.);
#5572=ADVANCED_FACE('',(#858,#442),#5322,.T.);
#5573=ADVANCED_FACE('',(#859,#443),#573,.T.);
#5574=ADVANCED_FACE('',(#860,#444),#574,.F.);
#5575=ADVANCED_FACE('',(#861,#445),#575,.T.);
#5576=ADVANCED_FACE('',(#862,#446),#576,.F.);
#5577=ADVANCED_FACE('',(#863),#5323,.T.);
#5578=ADVANCED_FACE('',(#864),#5324,.T.);
#5579=ADVANCED_FACE('',(#865),#5325,.T.);
#5580=ADVANCED_FACE('',(#866),#577,.T.);
#5581=ADVANCED_FACE('',(#867),#578,.F.);
#5582=ADVANCED_FACE('',(#868),#5326,.F.);
#5583=ADVANCED_FACE('',(#869),#5327,.T.);
#5584=ADVANCED_FACE('',(#870,#447),#579,.F.);
#5585=ADVANCED_FACE('',(#871),#580,.F.);
#5586=ADVANCED_FACE('',(#872),#581,.F.);
#5587=ADVANCED_FACE('',(#873),#5328,.T.);
#5588=ADVANCED_FACE('',(#874,#448),#582,.T.);
#5589=ADVANCED_FACE('',(#875),#5329,.F.);
#5590=ADVANCED_FACE('',(#876),#5330,.T.);
#5591=ADVANCED_FACE('',(#877,#449),#583,.T.);
#5592=ADVANCED_FACE('',(#878,#450),#584,.F.);
#5593=ADVANCED_FACE('',(#879),#5331,.F.);
#5594=ADVANCED_FACE('',(#880),#5332,.T.);
#5595=ADVANCED_FACE('',(#881,#451),#585,.T.);
#5596=ADVANCED_FACE('',(#882,#452),#586,.F.);
#5597=ADVANCED_FACE('',(#883),#5333,.F.);
#5598=ADVANCED_FACE('',(#884),#5334,.T.);
#5599=ADVANCED_FACE('',(#885,#453),#587,.T.);
#5600=ADVANCED_FACE('',(#886,#454),#588,.F.);
#5601=ADVANCED_FACE('',(#887),#589,.F.);
#5602=ADVANCED_FACE('',(#888),#590,.F.);
#5603=ADVANCED_FACE('',(#889),#591,.F.);
#5604=ADVANCED_FACE('',(#890),#592,.F.);
#5605=ADVANCED_FACE('',(#891),#593,.F.);
#5606=ADVANCED_FACE('',(#892),#594,.F.);
#5607=ADVANCED_FACE('',(#893),#595,.F.);
#5608=ADVANCED_FACE('',(#894),#596,.F.);
#5609=ADVANCED_FACE('',(#895),#597,.F.);
#5610=ADVANCED_FACE('',(#896),#598,.T.);
#5611=ADVANCED_FACE('',(#897),#207,.T.);
#5612=ADVANCED_FACE('',(#898),#5335,.T.);
#5613=ADVANCED_FACE('',(#899),#208,.T.);
#5614=ADVANCED_FACE('',(#900,#455),#599,.T.);
#5615=ADVANCED_FACE('',(#901),#209,.T.);
#5616=ADVANCED_FACE('',(#902),#5336,.T.);
#5617=ADVANCED_FACE('',(#903),#5337,.F.);
#5618=ADVANCED_FACE('',(#904),#5338,.F.);
#5619=ADVANCED_FACE('',(#905),#5339,.F.);
#5620=ADVANCED_FACE('',(#906),#5340,.F.);
#5621=ADVANCED_FACE('',(#907),#5341,.F.);
#5622=ADVANCED_FACE('',(#908),#5342,.F.);
#5623=ADVANCED_FACE('',(#909),#5343,.F.);
#5624=ADVANCED_FACE('',(#910),#5344,.F.);
#5625=ADVANCED_FACE('',(#911),#5345,.T.);
#5626=ADVANCED_FACE('',(#912),#5346,.T.);
#5627=ADVANCED_FACE('',(#913),#5347,.T.);
#5628=ADVANCED_FACE('',(#914,#456,#457,#458,#459),#600,.T.);
#5629=ADVANCED_FACE('',(#915),#5348,.T.);
#5630=ADVANCED_FACE('',(#916),#5349,.T.);
#5631=ADVANCED_FACE('',(#917),#601,.F.);
#5632=ADVANCED_FACE('',(#918),#602,.F.);
#5633=ADVANCED_FACE('',(#919),#603,.F.);
#5634=ADVANCED_FACE('',(#920),#604,.F.);
#5635=ADVANCED_FACE('',(#921),#605,.F.);
#5636=ADVANCED_FACE('',(#922,#460),#606,.F.);
#5637=ADVANCED_FACE('',(#923,#461),#607,.F.);
#5638=ADVANCED_FACE('',(#924),#608,.T.);
#5639=ADVANCED_FACE('',(#925),#5350,.F.);
#5640=ADVANCED_FACE('',(#926),#5351,.T.);
#5641=ADVANCED_FACE('',(#927),#609,.F.);
#5642=ADVANCED_FACE('',(#928),#5352,.T.);
#5643=ADVANCED_FACE('',(#929),#610,.F.);
#5644=ADVANCED_FACE('',(#930),#611,.F.);
#5645=ADVANCED_FACE('',(#931),#612,.F.);
#5646=ADVANCED_FACE('',(#932),#613,.F.);
#5647=ADVANCED_FACE('',(#933),#614,.F.);
#5648=ADVANCED_FACE('',(#934,#462),#615,.F.);
#5649=ADVANCED_FACE('',(#935),#616,.T.);
#5650=ADVANCED_FACE('',(#936),#5353,.F.);
#5651=ADVANCED_FACE('',(#937),#617,.F.);
#5652=ADVANCED_FACE('',(#938),#5354,.T.);
#5653=ADVANCED_FACE('',(#939),#618,.F.);
#5654=ADVANCED_FACE('',(#940),#619,.F.);
#5655=ADVANCED_FACE('',(#941),#620,.F.);
#5656=ADVANCED_FACE('',(#942),#621,.F.);
#5657=ADVANCED_FACE('',(#943),#622,.F.);
#5658=ADVANCED_FACE('',(#944,#463),#623,.F.);
#5659=ADVANCED_FACE('',(#945),#624,.T.);
#5660=ADVANCED_FACE('',(#946),#5355,.F.);
#5661=ADVANCED_FACE('',(#947),#625,.F.);
#5662=ADVANCED_FACE('',(#948),#5356,.T.);
#5663=ADVANCED_FACE('',(#949),#626,.F.);
#5664=ADVANCED_FACE('',(#950),#627,.F.);
#5665=ADVANCED_FACE('',(#951),#628,.F.);
#5666=ADVANCED_FACE('',(#952),#629,.F.);
#5667=ADVANCED_FACE('',(#953),#630,.T.);
#5668=ADVANCED_FACE('',(#954),#5357,.F.);
#5669=ADVANCED_FACE('',(#955),#631,.F.);
#5670=ADVANCED_FACE('',(#956),#632,.F.);
#5671=ADVANCED_FACE('',(#957,#464),#633,.F.);
#5672=ADVANCED_FACE('',(#958),#5358,.T.);
#5673=ADVANCED_FACE('',(#959),#634,.F.);
#5674=ADVANCED_FACE('',(#960),#5359,.F.);
#5675=ADVANCED_FACE('',(#961),#5360,.T.);
#5676=ADVANCED_FACE('',(#962,#465),#635,.T.);
#5677=ADVANCED_FACE('',(#963,#466),#636,.F.);
#5678=ADVANCED_FACE('',(#964),#637,.F.);
#5679=ADVANCED_FACE('',(#965),#5361,.F.);
#5680=ADVANCED_FACE('',(#966),#638,.F.);
#5681=ADVANCED_FACE('',(#967),#639,.F.);
#5682=ADVANCED_FACE('',(#968),#5362,.F.);
#5683=ADVANCED_FACE('',(#969),#640,.F.);
#5684=ADVANCED_FACE('',(#970,#467),#5363,.F.);
#5685=ADVANCED_FACE('',(#971,#468),#5364,.T.);
#5686=ADVANCED_FACE('',(#972,#469),#641,.T.);
#5687=ADVANCED_FACE('',(#973,#470),#642,.F.);
#5688=ADVANCED_FACE('',(#974),#643,.F.);
#5689=ADVANCED_FACE('',(#975),#644,.F.);
#5690=ADVANCED_FACE('',(#976),#645,.F.);
#5691=ADVANCED_FACE('',(#977),#646,.F.);
#5692=ADVANCED_FACE('',(#978),#647,.F.);
#5693=ADVANCED_FACE('',(#979),#648,.F.);
#5694=ADVANCED_FACE('',(#980),#649,.F.);
#5695=ADVANCED_FACE('',(#981),#650,.F.);
#5696=ADVANCED_FACE('',(#982,#471),#651,.T.);
#5697=ADVANCED_FACE('',(#983),#210,.T.);
#5698=ADVANCED_FACE('',(#984),#5365,.T.);
#5699=CLOSED_SHELL('',(#5366,#5367,#5368,#5369,#5370,#5371,#5372,#5373,
#5374,#5375));
#5700=CLOSED_SHELL('',(#5376,#5377,#5378,#5379,#5380,#5381));
#5701=CLOSED_SHELL('',(#5382,#5383,#5384,#5385,#5386,#5387));
#5702=CLOSED_SHELL('',(#5388,#5389,#5390,#5391,#5392,#5393,#5394,#5395,
#5396,#5397,#5398,#5399,#5400,#5401,#5402,#5403,#5404,#5405,#5406,#5407,
#5408,#5409,#5410,#5411,#5412,#5413,#5414,#5415,#5416,#5417,#5418,#5419,
#5420,#5421,#5422,#5423,#5424,#5425,#5426,#5427,#5428,#5429,#5430,#5431,
#5432,#5433,#5434,#5435,#5436,#5437));
#5703=CLOSED_SHELL('',(#5438,#5439,#5440,#5441,#5442,#5443,#5444,#5445,
#5446,#5447,#5448,#5449,#5450,#5451,#5452,#5453,#5454,#5455));
#5704=CLOSED_SHELL('',(#5456,#5457,#5458,#5459,#5460,#5461,#5462,#5463,
#5464,#5465,#5466,#5467,#5468,#5469,#5470,#5471,#5472,#5473));
#5705=CLOSED_SHELL('',(#5474,#5475,#5476,#5477,#5478,#5479,#5480,#5481,
#5482));
#5706=CLOSED_SHELL('',(#5483,#5484,#5485,#5486,#5487,#5488,#5489,#5490));
#5707=CLOSED_SHELL('',(#5491,#5492,#5493,#5494,#5495,#5496,#5497,#5498));
#5708=CLOSED_SHELL('',(#5499,#5500,#5501,#5502,#5503,#5504,#5505,#5506));
#5709=CLOSED_SHELL('',(#5507));
#5710=CLOSED_SHELL('',(#5508));
#5711=CLOSED_SHELL('',(#5509));
#5712=CLOSED_SHELL('',(#5510));
#5713=CLOSED_SHELL('',(#5511));
#5714=CLOSED_SHELL('',(#5512));
#5715=CLOSED_SHELL('',(#5513));
#5716=CLOSED_SHELL('',(#5514));
#5717=CLOSED_SHELL('',(#5515,#5516,#5517,#5518,#5519,#5520,#5521,#5522,
#5523,#5524,#5525,#5526,#5527,#5528,#5529,#5530,#5531,#5532,#5533));
#5718=CLOSED_SHELL('',(#5534,#5535,#5536,#5537));
#5719=CLOSED_SHELL('',(#5538,#5539,#5540,#5541));
#5720=CLOSED_SHELL('',(#5542,#5543,#5544,#5545,#5546,#5547,#5548,#5549,
#5550,#5551,#5552,#5553,#5554,#5555,#5556,#5557,#5558,#5559,#5560));
#5721=CLOSED_SHELL('',(#5561,#5562,#5563,#5564));
#5722=CLOSED_SHELL('',(#5565,#5566,#5567,#5568,#5569,#5570,#5571,#5572,
#5573,#5574));
#5723=CLOSED_SHELL('',(#5575,#5576,#5577,#5578,#5579,#5580,#5581));
#5724=CLOSED_SHELL('',(#5582,#5583,#5584,#5585,#5586,#5587,#5588));
#5725=CLOSED_SHELL('',(#5589,#5590,#5591,#5592));
#5726=CLOSED_SHELL('',(#5593,#5594,#5595,#5596));
#5727=CLOSED_SHELL('',(#5597,#5598,#5599,#5600));
#5728=CLOSED_SHELL('',(#5601,#5602,#5603,#5604,#5605,#5606,#5607,#5608));
#5729=CLOSED_SHELL('',(#5609,#5610,#5611,#5612,#5613,#5614,#5615,#5616));
#5730=CLOSED_SHELL('',(#5617,#5618,#5619,#5620,#5621,#5622,#5623,#5624,
#5625,#5626,#5627,#5628,#5629,#5630,#5631,#5632,#5633,#5634,#5635,#5636,
#5637,#5638,#5639,#5640,#5641,#5642,#5643,#5644,#5645,#5646,#5647,#5648,
#5649,#5650,#5651,#5652,#5653,#5654,#5655,#5656,#5657,#5658,#5659,#5660,
#5661,#5662,#5663,#5664,#5665,#5666,#5667,#5668,#5669,#5670,#5671,#5672,
#5673));
#5731=CLOSED_SHELL('',(#5674,#5675,#5676,#5677));
#5732=CLOSED_SHELL('',(#5678,#5679,#5680,#5681,#5682,#5683,#5684,#5685,
#5686,#5687));
#5733=CLOSED_SHELL('',(#5688,#5689,#5690,#5691,#5692,#5693,#5694,#5695,
#5696,#5697,#5698));
#5734=DERIVED_UNIT_ELEMENT(#5784,1.);
#5735=DERIVED_UNIT_ELEMENT(#10959,-3.);
#5736=DERIVED_UNIT_ELEMENT(#5784,1.);
#5737=DERIVED_UNIT_ELEMENT(#10959,-3.);
#5738=DERIVED_UNIT_ELEMENT(#5784,1.);
#5739=DERIVED_UNIT_ELEMENT(#10959,-3.);
#5740=DERIVED_UNIT_ELEMENT(#5784,1.);
#5741=DERIVED_UNIT_ELEMENT(#10959,-3.);
#5742=DERIVED_UNIT_ELEMENT(#5784,1.);
#5743=DERIVED_UNIT_ELEMENT(#10959,-3.);
#5744=DERIVED_UNIT_ELEMENT(#5784,1.);
#5745=DERIVED_UNIT_ELEMENT(#10959,-3.);
#5746=DERIVED_UNIT_ELEMENT(#5784,1.);
#5747=DERIVED_UNIT_ELEMENT(#10959,-3.);
#5748=DERIVED_UNIT_ELEMENT(#5784,1.);
#5749=DERIVED_UNIT_ELEMENT(#10959,-3.);
#5750=DERIVED_UNIT_ELEMENT(#5784,1.);
#5751=DERIVED_UNIT_ELEMENT(#10959,-3.);
#5752=DERIVED_UNIT_ELEMENT(#5784,1.);
#5753=DERIVED_UNIT_ELEMENT(#10959,-3.);
#5754=DERIVED_UNIT_ELEMENT(#5784,1.);
#5755=DERIVED_UNIT_ELEMENT(#10959,-3.);
#5756=DERIVED_UNIT_ELEMENT(#5784,1.);
#5757=DERIVED_UNIT_ELEMENT(#10959,-3.);
#5758=DERIVED_UNIT_ELEMENT(#5784,1.);
#5759=DERIVED_UNIT_ELEMENT(#10959,-3.);
#5760=DERIVED_UNIT_ELEMENT(#5784,1.);
#5761=DERIVED_UNIT_ELEMENT(#10959,-3.);
#5762=DERIVED_UNIT_ELEMENT(#5784,1.);
#5763=DERIVED_UNIT_ELEMENT(#10959,-3.);
#5764=DERIVED_UNIT_ELEMENT(#5784,1.);
#5765=DERIVED_UNIT_ELEMENT(#10959,-3.);
#5766=DERIVED_UNIT_ELEMENT(#5784,1.);
#5767=DERIVED_UNIT_ELEMENT(#10959,-3.);
#5768=DERIVED_UNIT_ELEMENT(#5784,1.);
#5769=DERIVED_UNIT_ELEMENT(#10959,-3.);
#5770=DERIVED_UNIT_ELEMENT(#5784,1.);
#5771=DERIVED_UNIT_ELEMENT(#10959,-3.);
#5772=DERIVED_UNIT_ELEMENT(#5784,1.);
#5773=DERIVED_UNIT_ELEMENT(#10959,-3.);
#5774=DERIVED_UNIT_ELEMENT(#5784,1.);
#5775=DERIVED_UNIT_ELEMENT(#10959,-3.);
#5776=DERIVED_UNIT_ELEMENT(#5784,1.);
#5777=DERIVED_UNIT_ELEMENT(#10959,-3.);
#5778=DERIVED_UNIT_ELEMENT(#5784,1.);
#5779=DERIVED_UNIT_ELEMENT(#10959,-3.);
#5780=DERIVED_UNIT_ELEMENT(#5784,1.);
#5781=DERIVED_UNIT_ELEMENT(#10959,-3.);
#5782=DERIVED_UNIT_ELEMENT(#5784,1.);
#5783=DERIVED_UNIT_ELEMENT(#10959,-3.);
#5784=(
MASS_UNIT()
NAMED_UNIT(*)
SI_UNIT(.KILO.,.GRAM.)
);
#5785=DERIVED_UNIT((#5734,#5735));
#5786=DERIVED_UNIT((#5736,#5737));
#5787=DERIVED_UNIT((#5738,#5739));
#5788=DERIVED_UNIT((#5740,#5741));
#5789=DERIVED_UNIT((#5742,#5743));
#5790=DERIVED_UNIT((#5744,#5745));
#5791=DERIVED_UNIT((#5746,#5747));
#5792=DERIVED_UNIT((#5748,#5749));
#5793=DERIVED_UNIT((#5750,#5751));
#5794=DERIVED_UNIT((#5752,#5753));
#5795=DERIVED_UNIT((#5754,#5755));
#5796=DERIVED_UNIT((#5756,#5757));
#5797=DERIVED_UNIT((#5758,#5759));
#5798=DERIVED_UNIT((#5760,#5761));
#5799=DERIVED_UNIT((#5762,#5763));
#5800=DERIVED_UNIT((#5764,#5765));
#5801=DERIVED_UNIT((#5766,#5767));
#5802=DERIVED_UNIT((#5768,#5769));
#5803=DERIVED_UNIT((#5770,#5771));
#5804=DERIVED_UNIT((#5772,#5773));
#5805=DERIVED_UNIT((#5774,#5775));
#5806=DERIVED_UNIT((#5776,#5777));
#5807=DERIVED_UNIT((#5778,#5779));
#5808=DERIVED_UNIT((#5780,#5781));
#5809=DERIVED_UNIT((#5782,#5783));
#5810=MEASURE_REPRESENTATION_ITEM('density measure',
POSITIVE_RATIO_MEASURE(7850.),#5785);
#5811=MEASURE_REPRESENTATION_ITEM('density measure',
POSITIVE_RATIO_MEASURE(7850.),#5786);
#5812=MEASURE_REPRESENTATION_ITEM('density measure',
POSITIVE_RATIO_MEASURE(7850.),#5787);
#5813=MEASURE_REPRESENTATION_ITEM('density measure',
POSITIVE_RATIO_MEASURE(7850.),#5788);
#5814=MEASURE_REPRESENTATION_ITEM('density measure',
POSITIVE_RATIO_MEASURE(7850.),#5789);
#5815=MEASURE_REPRESENTATION_ITEM('density measure',
POSITIVE_RATIO_MEASURE(7850.),#5790);
#5816=MEASURE_REPRESENTATION_ITEM('density measure',
POSITIVE_RATIO_MEASURE(7850.),#5791);
#5817=MEASURE_REPRESENTATION_ITEM('density measure',
POSITIVE_RATIO_MEASURE(7850.),#5792);
#5818=MEASURE_REPRESENTATION_ITEM('density measure',
POSITIVE_RATIO_MEASURE(7850.),#5793);
#5819=MEASURE_REPRESENTATION_ITEM('density measure',
POSITIVE_RATIO_MEASURE(7850.),#5794);
#5820=MEASURE_REPRESENTATION_ITEM('density measure',
POSITIVE_RATIO_MEASURE(7850.),#5795);
#5821=MEASURE_REPRESENTATION_ITEM('density measure',
POSITIVE_RATIO_MEASURE(7850.),#5796);
#5822=MEASURE_REPRESENTATION_ITEM('density measure',
POSITIVE_RATIO_MEASURE(7850.),#5797);
#5823=MEASURE_REPRESENTATION_ITEM('density measure',
POSITIVE_RATIO_MEASURE(7850.),#5798);
#5824=MEASURE_REPRESENTATION_ITEM('density measure',
POSITIVE_RATIO_MEASURE(7850.),#5799);
#5825=MEASURE_REPRESENTATION_ITEM('density measure',
POSITIVE_RATIO_MEASURE(7850.),#5800);
#5826=MEASURE_REPRESENTATION_ITEM('density measure',
POSITIVE_RATIO_MEASURE(7850.),#5801);
#5827=MEASURE_REPRESENTATION_ITEM('density measure',
POSITIVE_RATIO_MEASURE(7850.),#5802);
#5828=MEASURE_REPRESENTATION_ITEM('density measure',
POSITIVE_RATIO_MEASURE(7850.),#5803);
#5829=MEASURE_REPRESENTATION_ITEM('density measure',
POSITIVE_RATIO_MEASURE(7850.),#5804);
#5830=MEASURE_REPRESENTATION_ITEM('density measure',
POSITIVE_RATIO_MEASURE(7850.),#5805);
#5831=MEASURE_REPRESENTATION_ITEM('density measure',
POSITIVE_RATIO_MEASURE(7850.),#5806);
#5832=MEASURE_REPRESENTATION_ITEM('density measure',
POSITIVE_RATIO_MEASURE(7850.),#5807);
#5833=MEASURE_REPRESENTATION_ITEM('density measure',
POSITIVE_RATIO_MEASURE(7850.),#5808);
#5834=MEASURE_REPRESENTATION_ITEM('density measure',
POSITIVE_RATIO_MEASURE(7850.),#5809);
#5835=PROPERTY_DEFINITION_REPRESENTATION(#5960,#5885);
#5836=PROPERTY_DEFINITION_REPRESENTATION(#5961,#5886);
#5837=PROPERTY_DEFINITION_REPRESENTATION(#5962,#5887);
#5838=PROPERTY_DEFINITION_REPRESENTATION(#5963,#5888);
#5839=PROPERTY_DEFINITION_REPRESENTATION(#5964,#5889);
#5840=PROPERTY_DEFINITION_REPRESENTATION(#5965,#5890);
#5841=PROPERTY_DEFINITION_REPRESENTATION(#5966,#5891);
#5842=PROPERTY_DEFINITION_REPRESENTATION(#5967,#5892);
#5843=PROPERTY_DEFINITION_REPRESENTATION(#5968,#5893);
#5844=PROPERTY_DEFINITION_REPRESENTATION(#5969,#5894);
#5845=PROPERTY_DEFINITION_REPRESENTATION(#5970,#5895);
#5846=PROPERTY_DEFINITION_REPRESENTATION(#5971,#5896);
#5847=PROPERTY_DEFINITION_REPRESENTATION(#5972,#5897);
#5848=PROPERTY_DEFINITION_REPRESENTATION(#5973,#5898);
#5849=PROPERTY_DEFINITION_REPRESENTATION(#5974,#5899);
#5850=PROPERTY_DEFINITION_REPRESENTATION(#5975,#5900);
#5851=PROPERTY_DEFINITION_REPRESENTATION(#5976,#5901);
#5852=PROPERTY_DEFINITION_REPRESENTATION(#5977,#5902);
#5853=PROPERTY_DEFINITION_REPRESENTATION(#5978,#5903);
#5854=PROPERTY_DEFINITION_REPRESENTATION(#5979,#5904);
#5855=PROPERTY_DEFINITION_REPRESENTATION(#5980,#5905);
#5856=PROPERTY_DEFINITION_REPRESENTATION(#5981,#5906);
#5857=PROPERTY_DEFINITION_REPRESENTATION(#5982,#5907);
#5858=PROPERTY_DEFINITION_REPRESENTATION(#5983,#5908);
#5859=PROPERTY_DEFINITION_REPRESENTATION(#5984,#5909);
#5860=PROPERTY_DEFINITION_REPRESENTATION(#5985,#5910);
#5861=PROPERTY_DEFINITION_REPRESENTATION(#5986,#5911);
#5862=PROPERTY_DEFINITION_REPRESENTATION(#5987,#5912);
#5863=PROPERTY_DEFINITION_REPRESENTATION(#5988,#5913);
#5864=PROPERTY_DEFINITION_REPRESENTATION(#5989,#5914);
#5865=PROPERTY_DEFINITION_REPRESENTATION(#5990,#5915);
#5866=PROPERTY_DEFINITION_REPRESENTATION(#5991,#5916);
#5867=PROPERTY_DEFINITION_REPRESENTATION(#5992,#5917);
#5868=PROPERTY_DEFINITION_REPRESENTATION(#5993,#5918);
#5869=PROPERTY_DEFINITION_REPRESENTATION(#5994,#5919);
#5870=PROPERTY_DEFINITION_REPRESENTATION(#5995,#5920);
#5871=PROPERTY_DEFINITION_REPRESENTATION(#5996,#5921);
#5872=PROPERTY_DEFINITION_REPRESENTATION(#5997,#5922);
#5873=PROPERTY_DEFINITION_REPRESENTATION(#5998,#5923);
#5874=PROPERTY_DEFINITION_REPRESENTATION(#5999,#5924);
#5875=PROPERTY_DEFINITION_REPRESENTATION(#6000,#5925);
#5876=PROPERTY_DEFINITION_REPRESENTATION(#6001,#5926);
#5877=PROPERTY_DEFINITION_REPRESENTATION(#6002,#5927);
#5878=PROPERTY_DEFINITION_REPRESENTATION(#6003,#5928);
#5879=PROPERTY_DEFINITION_REPRESENTATION(#6004,#5929);
#5880=PROPERTY_DEFINITION_REPRESENTATION(#6005,#5930);
#5881=PROPERTY_DEFINITION_REPRESENTATION(#6006,#5931);
#5882=PROPERTY_DEFINITION_REPRESENTATION(#6007,#5932);
#5883=PROPERTY_DEFINITION_REPRESENTATION(#6008,#5933);
#5884=PROPERTY_DEFINITION_REPRESENTATION(#6009,#5934);
#5885=REPRESENTATION('material name',(#5935),#10929);
#5886=REPRESENTATION('density',(#5810),#10929);
#5887=REPRESENTATION('material name',(#5936),#10930);
#5888=REPRESENTATION('density',(#5811),#10930);
#5889=REPRESENTATION('material name',(#5937),#10931);
#5890=REPRESENTATION('density',(#5812),#10931);
#5891=REPRESENTATION('material name',(#5938),#10932);
#5892=REPRESENTATION('density',(#5813),#10932);
#5893=REPRESENTATION('material name',(#5939),#10933);
#5894=REPRESENTATION('density',(#5814),#10933);
#5895=REPRESENTATION('material name',(#5940),#10934);
#5896=REPRESENTATION('density',(#5815),#10934);
#5897=REPRESENTATION('material name',(#5941),#10935);
#5898=REPRESENTATION('density',(#5816),#10935);
#5899=REPRESENTATION('material name',(#5942),#10937);
#5900=REPRESENTATION('density',(#5817),#10937);
#5901=REPRESENTATION('material name',(#5943),#10938);
#5902=REPRESENTATION('density',(#5818),#10938);
#5903=REPRESENTATION('material name',(#5944),#10939);
#5904=REPRESENTATION('density',(#5819),#10939);
#5905=REPRESENTATION('material name',(#5945),#10940);
#5906=REPRESENTATION('density',(#5820),#10940);
#5907=REPRESENTATION('material name',(#5946),#10941);
#5908=REPRESENTATION('density',(#5821),#10941);
#5909=REPRESENTATION('material name',(#5947),#10943);
#5910=REPRESENTATION('density',(#5822),#10943);
#5911=REPRESENTATION('material name',(#5948),#10944);
#5912=REPRESENTATION('density',(#5823),#10944);
#5913=REPRESENTATION('material name',(#5949),#10945);
#5914=REPRESENTATION('density',(#5824),#10945);
#5915=REPRESENTATION('material name',(#5950),#10946);
#5916=REPRESENTATION('density',(#5825),#10946);
#5917=REPRESENTATION('material name',(#5951),#10947);
#5918=REPRESENTATION('density',(#5826),#10947);
#5919=REPRESENTATION('material name',(#5952),#10948);
#5920=REPRESENTATION('density',(#5827),#10948);
#5921=REPRESENTATION('material name',(#5953),#10949);
#5922=REPRESENTATION('density',(#5828),#10949);
#5923=REPRESENTATION('material name',(#5954),#10950);
#5924=REPRESENTATION('density',(#5829),#10950);
#5925=REPRESENTATION('material name',(#5955),#10951);
#5926=REPRESENTATION('density',(#5830),#10951);
#5927=REPRESENTATION('material name',(#5956),#10953);
#5928=REPRESENTATION('density',(#5831),#10953);
#5929=REPRESENTATION('material name',(#5957),#10954);
#5930=REPRESENTATION('density',(#5832),#10954);
#5931=REPRESENTATION('material name',(#5958),#10955);
#5932=REPRESENTATION('density',(#5833),#10955);
#5933=REPRESENTATION('material name',(#5959),#10956);
#5934=REPRESENTATION('density',(#5834),#10956);
#5935=DESCRIPTIVE_REPRESENTATION_ITEM('Steel','Steel');
#5936=DESCRIPTIVE_REPRESENTATION_ITEM('Steel','Steel');
#5937=DESCRIPTIVE_REPRESENTATION_ITEM('Steel','Steel');
#5938=DESCRIPTIVE_REPRESENTATION_ITEM('Steel','Steel');
#5939=DESCRIPTIVE_REPRESENTATION_ITEM('Steel','Steel');
#5940=DESCRIPTIVE_REPRESENTATION_ITEM('Steel','Steel');
#5941=DESCRIPTIVE_REPRESENTATION_ITEM('Steel','Steel');
#5942=DESCRIPTIVE_REPRESENTATION_ITEM('Steel','Steel');
#5943=DESCRIPTIVE_REPRESENTATION_ITEM('Steel','Steel');
#5944=DESCRIPTIVE_REPRESENTATION_ITEM('Steel','Steel');
#5945=DESCRIPTIVE_REPRESENTATION_ITEM('Steel','Steel');
#5946=DESCRIPTIVE_REPRESENTATION_ITEM('Steel','Steel');
#5947=DESCRIPTIVE_REPRESENTATION_ITEM('Steel','Steel');
#5948=DESCRIPTIVE_REPRESENTATION_ITEM('Steel','Steel');
#5949=DESCRIPTIVE_REPRESENTATION_ITEM('Steel','Steel');
#5950=DESCRIPTIVE_REPRESENTATION_ITEM('Steel','Steel');
#5951=DESCRIPTIVE_REPRESENTATION_ITEM('Steel','Steel');
#5952=DESCRIPTIVE_REPRESENTATION_ITEM('Steel','Steel');
#5953=DESCRIPTIVE_REPRESENTATION_ITEM('Steel','Steel');
#5954=DESCRIPTIVE_REPRESENTATION_ITEM('Steel','Steel');
#5955=DESCRIPTIVE_REPRESENTATION_ITEM('Steel','Steel');
#5956=DESCRIPTIVE_REPRESENTATION_ITEM('Steel','Steel');
#5957=DESCRIPTIVE_REPRESENTATION_ITEM('Steel','Steel');
#5958=DESCRIPTIVE_REPRESENTATION_ITEM('Steel','Steel');
#5959=DESCRIPTIVE_REPRESENTATION_ITEM('Steel','Steel');
#5960=PROPERTY_DEFINITION('material property','material name',#11097);
#5961=PROPERTY_DEFINITION('material property','density of part',#11097);
#5962=PROPERTY_DEFINITION('material property','material name',#11098);
#5963=PROPERTY_DEFINITION('material property','density of part',#11098);
#5964=PROPERTY_DEFINITION('material property','material name',#11099);
#5965=PROPERTY_DEFINITION('material property','density of part',#11099);
#5966=PROPERTY_DEFINITION('material property','material name',#11100);
#5967=PROPERTY_DEFINITION('material property','density of part',#11100);
#5968=PROPERTY_DEFINITION('material property','material name',#11101);
#5969=PROPERTY_DEFINITION('material property','density of part',#11101);
#5970=PROPERTY_DEFINITION('material property','material name',#11102);
#5971=PROPERTY_DEFINITION('material property','density of part',#11102);
#5972=PROPERTY_DEFINITION('material property','material name',#11103);
#5973=PROPERTY_DEFINITION('material property','density of part',#11103);
#5974=PROPERTY_DEFINITION('material property','material name',#11105);
#5975=PROPERTY_DEFINITION('material property','density of part',#11105);
#5976=PROPERTY_DEFINITION('material property','material name',#11106);
#5977=PROPERTY_DEFINITION('material property','density of part',#11106);
#5978=PROPERTY_DEFINITION('material property','material name',#11107);
#5979=PROPERTY_DEFINITION('material property','density of part',#11107);
#5980=PROPERTY_DEFINITION('material property','material name',#11108);
#5981=PROPERTY_DEFINITION('material property','density of part',#11108);
#5982=PROPERTY_DEFINITION('material property','material name',#11109);
#5983=PROPERTY_DEFINITION('material property','density of part',#11109);
#5984=PROPERTY_DEFINITION('material property','material name',#11111);
#5985=PROPERTY_DEFINITION('material property','density of part',#11111);
#5986=PROPERTY_DEFINITION('material property','material name',#11112);
#5987=PROPERTY_DEFINITION('material property','density of part',#11112);
#5988=PROPERTY_DEFINITION('material property','material name',#11113);
#5989=PROPERTY_DEFINITION('material property','density of part',#11113);
#5990=PROPERTY_DEFINITION('material property','material name',#11114);
#5991=PROPERTY_DEFINITION('material property','density of part',#11114);
#5992=PROPERTY_DEFINITION('material property','material name',#11115);
#5993=PROPERTY_DEFINITION('material property','density of part',#11115);
#5994=PROPERTY_DEFINITION('material property','material name',#11116);
#5995=PROPERTY_DEFINITION('material property','density of part',#11116);
#5996=PROPERTY_DEFINITION('material property','material name',#11117);
#5997=PROPERTY_DEFINITION('material property','density of part',#11117);
#5998=PROPERTY_DEFINITION('material property','material name',#11118);
#5999=PROPERTY_DEFINITION('material property','density of part',#11118);
#6000=PROPERTY_DEFINITION('material property','material name',#11119);
#6001=PROPERTY_DEFINITION('material property','density of part',#11119);
#6002=PROPERTY_DEFINITION('material property','material name',#11121);
#6003=PROPERTY_DEFINITION('material property','density of part',#11121);
#6004=PROPERTY_DEFINITION('material property','material name',#11122);
#6005=PROPERTY_DEFINITION('material property','density of part',#11122);
#6006=PROPERTY_DEFINITION('material property','material name',#11123);
#6007=PROPERTY_DEFINITION('material property','density of part',#11123);
#6008=PROPERTY_DEFINITION('material property','material name',#11124);
#6009=PROPERTY_DEFINITION('material property','density of part',#11124);
#6010=AXIS2_PLACEMENT_3D('',#8601,#6749,#6750);
#6011=AXIS2_PLACEMENT_3D('',#8602,#6751,#6752);
#6012=AXIS2_PLACEMENT_3D('',#8603,#6753,#6754);
#6013=AXIS2_PLACEMENT_3D('',#8604,#6755,#6756);
#6014=AXIS2_PLACEMENT_3D('',#8606,#6757,#6758);
#6015=AXIS2_PLACEMENT_3D('',#8609,#6760,#6761);
#6016=AXIS2_PLACEMENT_3D('',#8610,#6762,#6763);
#6017=AXIS2_PLACEMENT_3D('',#8612,#6764,#6765);
#6018=AXIS2_PLACEMENT_3D('',#8615,#6767,#6768);
#6019=AXIS2_PLACEMENT_3D('',#8616,#6769,#6770);
#6020=AXIS2_PLACEMENT_3D('',#8618,#6771,#6772);
#6021=AXIS2_PLACEMENT_3D('',#8621,#6774,#6775);
#6022=AXIS2_PLACEMENT_3D('',#8622,#6776,#6777);
#6023=AXIS2_PLACEMENT_3D('',#8624,#6778,#6779);
#6024=AXIS2_PLACEMENT_3D('',#8627,#6781,#6782);
#6025=AXIS2_PLACEMENT_3D('',#8628,#6783,#6784);
#6026=AXIS2_PLACEMENT_3D('',#8637,#6789,#6790);
#6027=AXIS2_PLACEMENT_3D('',#8643,#6794,#6795);
#6028=AXIS2_PLACEMENT_3D('',#8649,#6799,#6800);
#6029=AXIS2_PLACEMENT_3D('',#8652,#6803,#6804);
#6030=AXIS2_PLACEMENT_3D('',#8653,#6805,#6806);
#6031=AXIS2_PLACEMENT_3D('',#8654,#6807,#6808);
#6032=AXIS2_PLACEMENT_3D('',#8655,#6809,#6810);
#6033=AXIS2_PLACEMENT_3D('',#8664,#6815,#6816);
#6034=AXIS2_PLACEMENT_3D('',#8670,#6820,#6821);
#6035=AXIS2_PLACEMENT_3D('',#8676,#6825,#6826);
#6036=AXIS2_PLACEMENT_3D('',#8679,#6829,#6830);
#6037=AXIS2_PLACEMENT_3D('',#8680,#6831,#6832);
#6038=AXIS2_PLACEMENT_3D('',#8681,#6833,#6834);
#6039=AXIS2_PLACEMENT_3D('',#8682,#6835,#6836);
#6040=AXIS2_PLACEMENT_3D('',#8691,#6841,#6842);
#6041=AXIS2_PLACEMENT_3D('',#8697,#6846,#6847);
#6042=AXIS2_PLACEMENT_3D('',#8703,#6851,#6852);
#6043=AXIS2_PLACEMENT_3D('',#8706,#6855,#6856);
#6044=AXIS2_PLACEMENT_3D('',#8707,#6857,#6858);
#6045=AXIS2_PLACEMENT_3D('',#8708,#6859,#6860);
#6046=AXIS2_PLACEMENT_3D('',#8709,#6861,#6862);
#6047=AXIS2_PLACEMENT_3D('',#8711,#6863,#6864);
#6048=AXIS2_PLACEMENT_3D('',#8748,#6866,#6867);
#6049=AXIS2_PLACEMENT_3D('',#8750,#6868,#6869);
#6050=AXIS2_PLACEMENT_3D('',#8753,#6871,#6872);
#6051=AXIS2_PLACEMENT_3D('',#8754,#6873,#6874);
#6052=AXIS2_PLACEMENT_3D('',#8755,#6875,#6876);
#6053=AXIS2_PLACEMENT_3D('',#8757,#6877,#6878);
#6054=AXIS2_PLACEMENT_3D('',#8760,#6880,#6881);
#6055=AXIS2_PLACEMENT_3D('',#8761,#6882,#6883);
#6056=AXIS2_PLACEMENT_3D('',#8762,#6884,#6885);
#6057=AXIS2_PLACEMENT_3D('',#8764,#6886,#6887);
#6058=AXIS2_PLACEMENT_3D('',#8767,#6889,#6890);
#6059=AXIS2_PLACEMENT_3D('',#8768,#6891,#6892);
#6060=AXIS2_PLACEMENT_3D('',#8769,#6893,#6894);
#6061=AXIS2_PLACEMENT_3D('',#8771,#6895,#6896);
#6062=AXIS2_PLACEMENT_3D('',#8774,#6898,#6899);
#6063=AXIS2_PLACEMENT_3D('',#8775,#6900,#6901);
#6064=AXIS2_PLACEMENT_3D('',#8776,#6902,#6903);
#6065=AXIS2_PLACEMENT_3D('',#8778,#6904,#6905);
#6066=AXIS2_PLACEMENT_3D('',#8781,#6907,#6908);
#6067=AXIS2_PLACEMENT_3D('',#8782,#6909,#6910);
#6068=AXIS2_PLACEMENT_3D('',#8784,#6911,#6912);
#6069=AXIS2_PLACEMENT_3D('',#8785,#6913,#6914);
#6070=AXIS2_PLACEMENT_3D('',#8787,#6915,#6916);
#6071=AXIS2_PLACEMENT_3D('',#8789,#6918,#6919);
#6072=AXIS2_PLACEMENT_3D('',#8791,#6920,#6921);
#6073=AXIS2_PLACEMENT_3D('',#8828,#6923,#6924);
#6074=AXIS2_PLACEMENT_3D('',#8830,#6925,#6926);
#6075=AXIS2_PLACEMENT_3D('',#8833,#6928,#6929);
#6076=AXIS2_PLACEMENT_3D('',#8834,#6930,#6931);
#6077=AXIS2_PLACEMENT_3D('',#8835,#6932,#6933);
#6078=AXIS2_PLACEMENT_3D('',#8837,#6934,#6935);
#6079=AXIS2_PLACEMENT_3D('',#8840,#6937,#6938);
#6080=AXIS2_PLACEMENT_3D('',#8841,#6939,#6940);
#6081=AXIS2_PLACEMENT_3D('',#8842,#6941,#6942);
#6082=AXIS2_PLACEMENT_3D('',#8844,#6943,#6944);
#6083=AXIS2_PLACEMENT_3D('',#8847,#6946,#6947);
#6084=AXIS2_PLACEMENT_3D('',#8848,#6948,#6949);
#6085=AXIS2_PLACEMENT_3D('',#8849,#6950,#6951);
#6086=AXIS2_PLACEMENT_3D('',#8851,#6952,#6953);
#6087=AXIS2_PLACEMENT_3D('',#8854,#6955,#6956);
#6088=AXIS2_PLACEMENT_3D('',#8855,#6957,#6958);
#6089=AXIS2_PLACEMENT_3D('',#8856,#6959,#6960);
#6090=AXIS2_PLACEMENT_3D('',#8858,#6961,#6962);
#6091=AXIS2_PLACEMENT_3D('',#8861,#6964,#6965);
#6092=AXIS2_PLACEMENT_3D('',#8862,#6966,#6967);
#6093=AXIS2_PLACEMENT_3D('',#8864,#6968,#6969);
#6094=AXIS2_PLACEMENT_3D('',#8865,#6970,#6971);
#6095=AXIS2_PLACEMENT_3D('',#8867,#6972,#6973);
#6096=AXIS2_PLACEMENT_3D('',#8869,#6975,#6976);
#6097=AXIS2_PLACEMENT_3D('',#8874,#6978,#6979);
#6098=AXIS2_PLACEMENT_3D('',#8877,#6981,#6982);
#6099=AXIS2_PLACEMENT_3D('',#8878,#6983,#6984);
#6100=AXIS2_PLACEMENT_3D('',#8880,#6986,#6987);
#6101=AXIS2_PLACEMENT_3D('',#8882,#6989,#6990);
#6102=AXIS2_PLACEMENT_3D('',#8883,#6991,#6992);
#6103=AXIS2_PLACEMENT_3D('',#8885,#6993,#6994);
#6104=AXIS2_PLACEMENT_3D('',#8886,#6995,#6996);
#6105=AXIS2_PLACEMENT_3D('',#8891,#6998,#6999);
#6106=AXIS2_PLACEMENT_3D('',#8894,#7001,#7002);
#6107=AXIS2_PLACEMENT_3D('',#8895,#7003,#7004);
#6108=AXIS2_PLACEMENT_3D('',#8897,#7006,#7007);
#6109=AXIS2_PLACEMENT_3D('',#8899,#7009,#7010);
#6110=AXIS2_PLACEMENT_3D('',#8900,#7011,#7012);
#6111=AXIS2_PLACEMENT_3D('',#8902,#7013,#7014);
#6112=AXIS2_PLACEMENT_3D('',#8903,#7015,#7016);
#6113=AXIS2_PLACEMENT_3D('',#8908,#7018,#7019);
#6114=AXIS2_PLACEMENT_3D('',#8911,#7021,#7022);
#6115=AXIS2_PLACEMENT_3D('',#8912,#7023,#7024);
#6116=AXIS2_PLACEMENT_3D('',#8914,#7026,#7027);
#6117=AXIS2_PLACEMENT_3D('',#8916,#7029,#7030);
#6118=AXIS2_PLACEMENT_3D('',#8917,#7031,#7032);
#6119=AXIS2_PLACEMENT_3D('',#8919,#7033,#7034);
#6120=AXIS2_PLACEMENT_3D('',#8920,#7035,#7036);
#6121=AXIS2_PLACEMENT_3D('',#8925,#7038,#7039);
#6122=AXIS2_PLACEMENT_3D('',#8928,#7041,#7042);
#6123=AXIS2_PLACEMENT_3D('',#8929,#7043,#7044);
#6124=AXIS2_PLACEMENT_3D('',#8931,#7046,#7047);
#6125=AXIS2_PLACEMENT_3D('',#8933,#7049,#7050);
#6126=AXIS2_PLACEMENT_3D('',#8934,#7051,#7052);
#6127=AXIS2_PLACEMENT_3D('',#8936,#7053,#7054);
#6128=AXIS2_PLACEMENT_3D('',#8937,#7055,#7056);
#6129=AXIS2_PLACEMENT_3D('',#8941,#7059,#7060);
#6130=AXIS2_PLACEMENT_3D('',#8945,#7063,#7064);
#6131=AXIS2_PLACEMENT_3D('',#8949,#7067,#7068);
#6132=AXIS2_PLACEMENT_3D('',#8954,#7073,#7074);
#6133=AXIS2_PLACEMENT_3D('',#8958,#7077,#7078);
#6134=AXIS2_PLACEMENT_3D('',#8960,#7079,#7080);
#6135=AXIS2_PLACEMENT_3D('',#8962,#7082,#7083);
#6136=AXIS2_PLACEMENT_3D('',#8964,#7084,#7085);
#6137=AXIS2_PLACEMENT_3D('',#8966,#7087,#7088);
#6138=AXIS2_PLACEMENT_3D('',#8968,#7089,#7090);
#6139=AXIS2_PLACEMENT_3D('',#8970,#7092,#7093);
#6140=AXIS2_PLACEMENT_3D('',#8972,#7094,#7095);
#6141=AXIS2_PLACEMENT_3D('',#8974,#7097,#7098);
#6142=AXIS2_PLACEMENT_3D('',#8980,#7102,#7103);
#6143=AXIS2_PLACEMENT_3D('',#8984,#7106,#7107);
#6144=AXIS2_PLACEMENT_3D('',#8988,#7110,#7111);
#6145=AXIS2_PLACEMENT_3D('',#8990,#7113,#7114);
#6146=AXIS2_PLACEMENT_3D('',#8991,#7115,#7116);
#6147=AXIS2_PLACEMENT_3D('',#8992,#7117,#7118);
#6148=AXIS2_PLACEMENT_3D('',#8997,#7120,#7121);
#6149=AXIS2_PLACEMENT_3D('',#9000,#7123,#7124);
#6150=AXIS2_PLACEMENT_3D('',#9001,#7125,#7126);
#6151=AXIS2_PLACEMENT_3D('',#9003,#7127,#7128);
#6152=AXIS2_PLACEMENT_3D('',#9004,#7129,#7130);
#6153=AXIS2_PLACEMENT_3D('',#9006,#7131,#7132);
#6154=AXIS2_PLACEMENT_3D('',#9007,#7133,#7134);
#6155=AXIS2_PLACEMENT_3D('',#9010,#7135,#7136);
#6156=AXIS2_PLACEMENT_3D('',#9011,#7137,#7138);
#6157=AXIS2_PLACEMENT_3D('',#9013,#7139,#7140);
#6158=AXIS2_PLACEMENT_3D('',#9014,#7141,#7142);
#6159=AXIS2_PLACEMENT_3D('',#9018,#7144,#7145);
#6160=AXIS2_PLACEMENT_3D('',#9020,#7147,#7148);
#6161=AXIS2_PLACEMENT_3D('',#9023,#7149,#7150);
#6162=AXIS2_PLACEMENT_3D('',#9024,#7151,#7152);
#6163=AXIS2_PLACEMENT_3D('',#9026,#7153,#7154);
#6164=AXIS2_PLACEMENT_3D('',#9027,#7155,#7156);
#6165=AXIS2_PLACEMENT_3D('',#9031,#7158,#7159);
#6166=AXIS2_PLACEMENT_3D('',#9033,#7161,#7162);
#6167=AXIS2_PLACEMENT_3D('',#9036,#7163,#7164);
#6168=AXIS2_PLACEMENT_3D('',#9037,#7165,#7166);
#6169=AXIS2_PLACEMENT_3D('',#9039,#7167,#7168);
#6170=AXIS2_PLACEMENT_3D('',#9040,#7169,#7170);
#6171=AXIS2_PLACEMENT_3D('',#9044,#7172,#7173);
#6172=AXIS2_PLACEMENT_3D('',#9046,#7175,#7176);
#6173=AXIS2_PLACEMENT_3D('',#9047,#7177,#7178);
#6174=AXIS2_PLACEMENT_3D('',#9048,#7179,#7180);
#6175=AXIS2_PLACEMENT_3D('',#9049,#7181,#7182);
#6176=AXIS2_PLACEMENT_3D('',#9050,#7183,#7184);
#6177=AXIS2_PLACEMENT_3D('',#9052,#7185,#7186);
#6178=AXIS2_PLACEMENT_3D('',#9053,#7187,#7188);
#6179=AXIS2_PLACEMENT_3D('',#9055,#7189,#7190);
#6180=AXIS2_PLACEMENT_3D('',#9057,#7192,#7193);
#6181=AXIS2_PLACEMENT_3D('',#9059,#7194,#7195);
#6182=AXIS2_PLACEMENT_3D('',#9061,#7197,#7198);
#6183=AXIS2_PLACEMENT_3D('',#9063,#7199,#7200);
#6184=AXIS2_PLACEMENT_3D('',#9065,#7202,#7203);
#6185=AXIS2_PLACEMENT_3D('',#9067,#7204,#7205);
#6186=AXIS2_PLACEMENT_3D('',#9069,#7207,#7208);
#6187=AXIS2_PLACEMENT_3D('',#9071,#7209,#7210);
#6188=AXIS2_PLACEMENT_3D('',#9074,#7212,#7213);
#6189=AXIS2_PLACEMENT_3D('',#9075,#7214,#7215);
#6190=AXIS2_PLACEMENT_3D('',#9077,#7216,#7217);
#6191=AXIS2_PLACEMENT_3D('',#9078,#7218,#7219);
#6192=AXIS2_PLACEMENT_3D('',#9080,#7221,#7222);
#6193=AXIS2_PLACEMENT_3D('',#9083,#7224,#7225);
#6194=AXIS2_PLACEMENT_3D('',#9084,#7226,#7227);
#6195=AXIS2_PLACEMENT_3D('',#9085,#7228,#7229);
#6196=AXIS2_PLACEMENT_3D('',#9086,#7230,#7231);
#6197=AXIS2_PLACEMENT_3D('',#9091,#7233,#7234);
#6198=AXIS2_PLACEMENT_3D('',#9094,#7236,#7237);
#6199=AXIS2_PLACEMENT_3D('',#9095,#7238,#7239);
#6200=AXIS2_PLACEMENT_3D('',#9097,#7240,#7241);
#6201=AXIS2_PLACEMENT_3D('',#9098,#7242,#7243);
#6202=AXIS2_PLACEMENT_3D('',#9100,#7244,#7245);
#6203=AXIS2_PLACEMENT_3D('',#9101,#7246,#7247);
#6204=AXIS2_PLACEMENT_3D('',#9104,#7248,#7249);
#6205=AXIS2_PLACEMENT_3D('',#9105,#7250,#7251);
#6206=AXIS2_PLACEMENT_3D('',#9107,#7252,#7253);
#6207=AXIS2_PLACEMENT_3D('',#9108,#7254,#7255);
#6208=AXIS2_PLACEMENT_3D('',#9112,#7257,#7258);
#6209=AXIS2_PLACEMENT_3D('',#9114,#7260,#7261);
#6210=AXIS2_PLACEMENT_3D('',#9117,#7262,#7263);
#6211=AXIS2_PLACEMENT_3D('',#9118,#7264,#7265);
#6212=AXIS2_PLACEMENT_3D('',#9120,#7266,#7267);
#6213=AXIS2_PLACEMENT_3D('',#9121,#7268,#7269);
#6214=AXIS2_PLACEMENT_3D('',#9125,#7271,#7272);
#6215=AXIS2_PLACEMENT_3D('',#9127,#7274,#7275);
#6216=AXIS2_PLACEMENT_3D('',#9130,#7276,#7277);
#6217=AXIS2_PLACEMENT_3D('',#9131,#7278,#7279);
#6218=AXIS2_PLACEMENT_3D('',#9133,#7280,#7281);
#6219=AXIS2_PLACEMENT_3D('',#9134,#7282,#7283);
#6220=AXIS2_PLACEMENT_3D('',#9138,#7285,#7286);
#6221=AXIS2_PLACEMENT_3D('',#9140,#7288,#7289);
#6222=AXIS2_PLACEMENT_3D('',#9141,#7290,#7291);
#6223=AXIS2_PLACEMENT_3D('',#9142,#7292,#7293);
#6224=AXIS2_PLACEMENT_3D('',#9143,#7294,#7295);
#6225=AXIS2_PLACEMENT_3D('',#9144,#7296,#7297);
#6226=AXIS2_PLACEMENT_3D('',#9146,#7298,#7299);
#6227=AXIS2_PLACEMENT_3D('',#9147,#7300,#7301);
#6228=AXIS2_PLACEMENT_3D('',#9149,#7302,#7303);
#6229=AXIS2_PLACEMENT_3D('',#9151,#7305,#7306);
#6230=AXIS2_PLACEMENT_3D('',#9153,#7307,#7308);
#6231=AXIS2_PLACEMENT_3D('',#9155,#7310,#7311);
#6232=AXIS2_PLACEMENT_3D('',#9157,#7312,#7313);
#6233=AXIS2_PLACEMENT_3D('',#9159,#7315,#7316);
#6234=AXIS2_PLACEMENT_3D('',#9161,#7317,#7318);
#6235=AXIS2_PLACEMENT_3D('',#9163,#7320,#7321);
#6236=AXIS2_PLACEMENT_3D('',#9165,#7322,#7323);
#6237=AXIS2_PLACEMENT_3D('',#9168,#7325,#7326);
#6238=AXIS2_PLACEMENT_3D('',#9169,#7327,#7328);
#6239=AXIS2_PLACEMENT_3D('',#9171,#7329,#7330);
#6240=AXIS2_PLACEMENT_3D('',#9172,#7331,#7332);
#6241=AXIS2_PLACEMENT_3D('',#9174,#7334,#7335);
#6242=AXIS2_PLACEMENT_3D('',#9177,#7337,#7338);
#6243=AXIS2_PLACEMENT_3D('',#9178,#7339,#7340);
#6244=AXIS2_PLACEMENT_3D('',#9179,#7341,#7342);
#6245=AXIS2_PLACEMENT_3D('',#9180,#7343,#7344);
#6246=AXIS2_PLACEMENT_3D('',#9182,#7345,#7346);
#6247=AXIS2_PLACEMENT_3D('',#9183,#7347,#7348);
#6248=AXIS2_PLACEMENT_3D('',#9185,#7349,#7350);
#6249=AXIS2_PLACEMENT_3D('',#9187,#7352,#7353);
#6250=AXIS2_PLACEMENT_3D('',#9189,#7354,#7355);
#6251=AXIS2_PLACEMENT_3D('',#9191,#7357,#7358);
#6252=AXIS2_PLACEMENT_3D('',#9193,#7359,#7360);
#6253=AXIS2_PLACEMENT_3D('',#9195,#7362,#7363);
#6254=AXIS2_PLACEMENT_3D('',#9197,#7364,#7365);
#6255=AXIS2_PLACEMENT_3D('',#9198,#7366,#7367);
#6256=AXIS2_PLACEMENT_3D('',#9200,#7368,#7369);
#6257=AXIS2_PLACEMENT_3D('',#9202,#7371,#7372);
#6258=AXIS2_PLACEMENT_3D('',#9204,#7373,#7374);
#6259=AXIS2_PLACEMENT_3D('',#9206,#7376,#7377);
#6260=AXIS2_PLACEMENT_3D('',#9208,#7378,#7379);
#6261=AXIS2_PLACEMENT_3D('',#9210,#7381,#7382);
#6262=AXIS2_PLACEMENT_3D('',#9211,#7383,#7384);
#6263=AXIS2_PLACEMENT_3D('',#9220,#7389,#7390);
#6264=AXIS2_PLACEMENT_3D('',#9226,#7394,#7395);
#6265=AXIS2_PLACEMENT_3D('',#9232,#7399,#7400);
#6266=AXIS2_PLACEMENT_3D('',#9238,#7404,#7405);
#6267=AXIS2_PLACEMENT_3D('',#9244,#7409,#7410);
#6268=AXIS2_PLACEMENT_3D('',#9247,#7413,#7414);
#6269=AXIS2_PLACEMENT_3D('',#9248,#7415,#7416);
#6270=AXIS2_PLACEMENT_3D('',#9249,#7417,#7418);
#6271=AXIS2_PLACEMENT_3D('',#9250,#7419,#7420);
#6272=AXIS2_PLACEMENT_3D('',#9251,#7421,#7422);
#6273=AXIS2_PLACEMENT_3D('',#9254,#7423,#7424);
#6274=AXIS2_PLACEMENT_3D('',#9255,#7425,#7426);
#6275=AXIS2_PLACEMENT_3D('',#9257,#7427,#7428);
#6276=AXIS2_PLACEMENT_3D('',#9259,#7429,#7430);
#6277=AXIS2_PLACEMENT_3D('',#9260,#7431,#7432);
#6278=AXIS2_PLACEMENT_3D('',#9261,#7433,#7434);
#6279=AXIS2_PLACEMENT_3D('',#9264,#7436,#7437);
#6280=AXIS2_PLACEMENT_3D('',#9265,#7438,#7439);
#6281=AXIS2_PLACEMENT_3D('',#9267,#7440,#7441);
#6282=AXIS2_PLACEMENT_3D('',#9270,#7443,#7444);
#6283=AXIS2_PLACEMENT_3D('',#9271,#7445,#7446);
#6284=AXIS2_PLACEMENT_3D('',#9274,#7448,#7449);
#6285=AXIS2_PLACEMENT_3D('',#9275,#7450,#7451);
#6286=AXIS2_PLACEMENT_3D('',#9276,#7452,#7453);
#6287=AXIS2_PLACEMENT_3D('',#9278,#7454,#7455);
#6288=AXIS2_PLACEMENT_3D('',#9280,#7457,#7458);
#6289=AXIS2_PLACEMENT_3D('',#9282,#7459,#7460);
#6290=AXIS2_PLACEMENT_3D('',#9283,#7461,#7462);
#6291=AXIS2_PLACEMENT_3D('',#9285,#7464,#7465);
#6292=AXIS2_PLACEMENT_3D('',#9286,#7466,#7467);
#6293=AXIS2_PLACEMENT_3D('',#9289,#7468,#7469);
#6294=AXIS2_PLACEMENT_3D('',#9290,#7470,#7471);
#6295=AXIS2_PLACEMENT_3D('',#9292,#7472,#7473);
#6296=AXIS2_PLACEMENT_3D('',#9294,#7474,#7475);
#6297=AXIS2_PLACEMENT_3D('',#9295,#7476,#7477);
#6298=AXIS2_PLACEMENT_3D('',#9296,#7478,#7479);
#6299=AXIS2_PLACEMENT_3D('',#9298,#7480,#7481);
#6300=AXIS2_PLACEMENT_3D('',#9300,#7483,#7484);
#6301=AXIS2_PLACEMENT_3D('',#9302,#7485,#7486);
#6302=AXIS2_PLACEMENT_3D('',#9304,#7487,#7488);
#6303=AXIS2_PLACEMENT_3D('',#9305,#7489,#7490);
#6304=AXIS2_PLACEMENT_3D('',#9307,#7491,#7492);
#6305=AXIS2_PLACEMENT_3D('',#9309,#7494,#7495);
#6306=AXIS2_PLACEMENT_3D('',#9311,#7496,#7497);
#6307=AXIS2_PLACEMENT_3D('',#9313,#7499,#7500);
#6308=AXIS2_PLACEMENT_3D('',#9315,#7501,#7502);
#6309=AXIS2_PLACEMENT_3D('',#9317,#7504,#7505);
#6310=AXIS2_PLACEMENT_3D('',#9318,#7506,#7507);
#6311=AXIS2_PLACEMENT_3D('',#9320,#7509,#7510);
#6312=AXIS2_PLACEMENT_3D('',#9321,#7511,#7512);
#6313=AXIS2_PLACEMENT_3D('',#9324,#7513,#7514);
#6314=AXIS2_PLACEMENT_3D('',#9325,#7515,#7516);
#6315=AXIS2_PLACEMENT_3D('',#9328,#7517,#7518);
#6316=AXIS2_PLACEMENT_3D('',#9329,#7519,#7520);
#6317=AXIS2_PLACEMENT_3D('',#9332,#7521,#7522);
#6318=AXIS2_PLACEMENT_3D('',#9333,#7523,#7524);
#6319=AXIS2_PLACEMENT_3D('',#9336,#7525,#7526);
#6320=AXIS2_PLACEMENT_3D('',#9337,#7527,#7528);
#6321=AXIS2_PLACEMENT_3D('',#9340,#7529,#7530);
#6322=AXIS2_PLACEMENT_3D('',#9341,#7531,#7532);
#6323=AXIS2_PLACEMENT_3D('',#9344,#7533,#7534);
#6324=AXIS2_PLACEMENT_3D('',#9345,#7535,#7536);
#6325=AXIS2_PLACEMENT_3D('',#9348,#7537,#7538);
#6326=AXIS2_PLACEMENT_3D('',#9349,#7539,#7540);
#6327=AXIS2_PLACEMENT_3D('',#9352,#7541,#7542);
#6328=AXIS2_PLACEMENT_3D('',#9353,#7543,#7544);
#6329=AXIS2_PLACEMENT_3D('',#9354,#7545,#7546);
#6330=AXIS2_PLACEMENT_3D('',#9380,#7547,#7548);
#6331=AXIS2_PLACEMENT_3D('',#9404,#7549,#7550);
#6332=AXIS2_PLACEMENT_3D('',#9405,#7551,#7552);
#6333=AXIS2_PLACEMENT_3D('',#9407,#7553,#7554);
#6334=AXIS2_PLACEMENT_3D('',#9432,#7555,#7556);
#6335=AXIS2_PLACEMENT_3D('',#9457,#7557,#7558);
#6336=AXIS2_PLACEMENT_3D('',#9473,#7560,#7561);
#6337=AXIS2_PLACEMENT_3D('',#9488,#7562,#7563);
#6338=AXIS2_PLACEMENT_3D('',#9513,#7564,#7565);
#6339=AXIS2_PLACEMENT_3D('',#9538,#7566,#7567);
#6340=AXIS2_PLACEMENT_3D('',#9563,#7568,#7569);
#6341=AXIS2_PLACEMENT_3D('',#9587,#7570,#7571);
#6342=AXIS2_PLACEMENT_3D('',#9588,#7572,#7573);
#6343=AXIS2_PLACEMENT_3D('',#9590,#7574,#7575);
#6344=AXIS2_PLACEMENT_3D('',#9591,#7576,#7577);
#6345=AXIS2_PLACEMENT_3D('',#9592,#7578,#7579);
#6346=AXIS2_PLACEMENT_3D('',#9616,#7580,#7581);
#6347=AXIS2_PLACEMENT_3D('',#9617,#7582,#7583);
#6348=AXIS2_PLACEMENT_3D('',#9619,#7584,#7585);
#6349=AXIS2_PLACEMENT_3D('',#9620,#7586,#7587);
#6350=AXIS2_PLACEMENT_3D('',#9621,#7588,#7589);
#6351=AXIS2_PLACEMENT_3D('',#9645,#7590,#7591);
#6352=AXIS2_PLACEMENT_3D('',#9646,#7592,#7593);
#6353=AXIS2_PLACEMENT_3D('',#9648,#7594,#7595);
#6354=AXIS2_PLACEMENT_3D('',#9649,#7596,#7597);
#6355=AXIS2_PLACEMENT_3D('',#9650,#7598,#7599);
#6356=AXIS2_PLACEMENT_3D('',#9665,#7600,#7601);
#6357=AXIS2_PLACEMENT_3D('',#9678,#7602,#7603);
#6358=AXIS2_PLACEMENT_3D('',#9680,#7604,#7605);
#6359=AXIS2_PLACEMENT_3D('',#9681,#7606,#7607);
#6360=AXIS2_PLACEMENT_3D('',#9682,#7608,#7609);
#6361=AXIS2_PLACEMENT_3D('',#9706,#7610,#7611);
#6362=AXIS2_PLACEMENT_3D('',#9707,#7612,#7613);
#6363=AXIS2_PLACEMENT_3D('',#9709,#7614,#7615);
#6364=AXIS2_PLACEMENT_3D('',#9710,#7616,#7617);
#6365=AXIS2_PLACEMENT_3D('',#9711,#7618,#7619);
#6366=AXIS2_PLACEMENT_3D('',#9735,#7620,#7621);
#6367=AXIS2_PLACEMENT_3D('',#9736,#7622,#7623);
#6368=AXIS2_PLACEMENT_3D('',#9738,#7624,#7625);
#6369=AXIS2_PLACEMENT_3D('',#9739,#7626,#7627);
#6370=AXIS2_PLACEMENT_3D('',#9740,#7628,#7629);
#6371=AXIS2_PLACEMENT_3D('',#9764,#7630,#7631);
#6372=AXIS2_PLACEMENT_3D('',#9765,#7632,#7633);
#6373=AXIS2_PLACEMENT_3D('',#9767,#7634,#7635);
#6374=AXIS2_PLACEMENT_3D('',#9770,#7637,#7638);
#6375=AXIS2_PLACEMENT_3D('',#9794,#7639,#7640);
#6376=AXIS2_PLACEMENT_3D('',#9795,#7641,#7642);
#6377=AXIS2_PLACEMENT_3D('',#9796,#7643,#7644);
#6378=AXIS2_PLACEMENT_3D('',#9797,#7645,#7646);
#6379=AXIS2_PLACEMENT_3D('',#9798,#7647,#7648);
#6380=AXIS2_PLACEMENT_3D('',#9799,#7649,#7650);
#6381=AXIS2_PLACEMENT_3D('',#9800,#7651,#7652);
#6382=AXIS2_PLACEMENT_3D('',#9801,#7653,#7654);
#6383=AXIS2_PLACEMENT_3D('',#9802,#7655,#7656);
#6384=AXIS2_PLACEMENT_3D('',#9804,#7657,#7658);
#6385=AXIS2_PLACEMENT_3D('',#9806,#7659,#7660);
#6386=AXIS2_PLACEMENT_3D('',#9807,#7661,#7662);
#6387=AXIS2_PLACEMENT_3D('',#9809,#7663,#7664);
#6388=AXIS2_PLACEMENT_3D('',#9811,#7666,#7667);
#6389=AXIS2_PLACEMENT_3D('',#9813,#7668,#7669);
#6390=AXIS2_PLACEMENT_3D('',#9814,#7670,#7671);
#6391=AXIS2_PLACEMENT_3D('',#9816,#7673,#7674);
#6392=AXIS2_PLACEMENT_3D('',#9818,#7675,#7676);
#6393=AXIS2_PLACEMENT_3D('',#9820,#7677,#7678);
#6394=AXIS2_PLACEMENT_3D('',#9821,#7679,#7680);
#6395=AXIS2_PLACEMENT_3D('',#9823,#7681,#7682);
#6396=AXIS2_PLACEMENT_3D('',#9825,#7684,#7685);
#6397=AXIS2_PLACEMENT_3D('',#9827,#7686,#7687);
#6398=AXIS2_PLACEMENT_3D('',#9828,#7688,#7689);
#6399=AXIS2_PLACEMENT_3D('',#9830,#7691,#7692);
#6400=AXIS2_PLACEMENT_3D('',#9831,#7693,#7694);
#6401=AXIS2_PLACEMENT_3D('',#9832,#7695,#7696);
#6402=AXIS2_PLACEMENT_3D('',#9833,#7697,#7698);
#6403=AXIS2_PLACEMENT_3D('',#9834,#7699,#7700);
#6404=AXIS2_PLACEMENT_3D('',#9835,#7701,#7702);
#6405=AXIS2_PLACEMENT_3D('',#9836,#7703,#7704);
#6406=AXIS2_PLACEMENT_3D('',#9837,#7705,#7706);
#6407=AXIS2_PLACEMENT_3D('',#9839,#7707,#7708);
#6408=AXIS2_PLACEMENT_3D('',#9842,#7710,#7711);
#6409=AXIS2_PLACEMENT_3D('',#9843,#7712,#7713);
#6410=AXIS2_PLACEMENT_3D('',#9844,#7714,#7715);
#6411=AXIS2_PLACEMENT_3D('',#9846,#7716,#7717);
#6412=AXIS2_PLACEMENT_3D('',#9849,#7719,#7720);
#6413=AXIS2_PLACEMENT_3D('',#9850,#7721,#7722);
#6414=AXIS2_PLACEMENT_3D('',#9855,#7724,#7725);
#6415=AXIS2_PLACEMENT_3D('',#9858,#7727,#7728);
#6416=AXIS2_PLACEMENT_3D('',#9859,#7729,#7730);
#6417=AXIS2_PLACEMENT_3D('',#9863,#7732,#7733);
#6418=AXIS2_PLACEMENT_3D('',#9871,#7737,#7738);
#6419=AXIS2_PLACEMENT_3D('',#9874,#7740,#7741);
#6420=AXIS2_PLACEMENT_3D('',#9875,#7742,#7743);
#6421=AXIS2_PLACEMENT_3D('',#9879,#7746,#7747);
#6422=AXIS2_PLACEMENT_3D('',#9883,#7750,#7751);
#6423=AXIS2_PLACEMENT_3D('',#9889,#7755,#7756);
#6424=AXIS2_PLACEMENT_3D('',#9895,#7760,#7761);
#6425=AXIS2_PLACEMENT_3D('',#9897,#7763,#7764);
#6426=AXIS2_PLACEMENT_3D('',#9898,#7765,#7766);
#6427=AXIS2_PLACEMENT_3D('',#9899,#7767,#7768);
#6428=AXIS2_PLACEMENT_3D('',#9901,#7769,#7770);
#6429=AXIS2_PLACEMENT_3D('',#9902,#7771,#7772);
#6430=AXIS2_PLACEMENT_3D('',#9903,#7773,#7774);
#6431=AXIS2_PLACEMENT_3D('',#9904,#7775,#7776);
#6432=AXIS2_PLACEMENT_3D('',#9906,#7777,#7778);
#6433=AXIS2_PLACEMENT_3D('',#9908,#7779,#7780);
#6434=AXIS2_PLACEMENT_3D('',#9909,#7781,#7782);
#6435=AXIS2_PLACEMENT_3D('',#9911,#7784,#7785);
#6436=AXIS2_PLACEMENT_3D('',#9914,#7787,#7788);
#6437=AXIS2_PLACEMENT_3D('',#9915,#7789,#7790);
#6438=AXIS2_PLACEMENT_3D('',#9917,#7791,#7792);
#6439=AXIS2_PLACEMENT_3D('',#9919,#7794,#7795);
#6440=AXIS2_PLACEMENT_3D('',#9920,#7796,#7797);
#6441=AXIS2_PLACEMENT_3D('',#9921,#7798,#7799);
#6442=AXIS2_PLACEMENT_3D('',#9922,#7800,#7801);
#6443=AXIS2_PLACEMENT_3D('',#9924,#7802,#7803);
#6444=AXIS2_PLACEMENT_3D('',#9927,#7805,#7806);
#6445=AXIS2_PLACEMENT_3D('',#9928,#7807,#7808);
#6446=AXIS2_PLACEMENT_3D('',#9930,#7809,#7810);
#6447=AXIS2_PLACEMENT_3D('',#9933,#7812,#7813);
#6448=AXIS2_PLACEMENT_3D('',#9934,#7814,#7815);
#6449=AXIS2_PLACEMENT_3D('',#9935,#7816,#7817);
#6450=AXIS2_PLACEMENT_3D('',#9936,#7818,#7819);
#6451=AXIS2_PLACEMENT_3D('',#9937,#7820,#7821);
#6452=AXIS2_PLACEMENT_3D('',#9942,#7823,#7824);
#6453=AXIS2_PLACEMENT_3D('',#9943,#7825,#7826);
#6454=AXIS2_PLACEMENT_3D('',#9944,#7827,#7828);
#6455=AXIS2_PLACEMENT_3D('',#9997,#7830,#7831);
#6456=AXIS2_PLACEMENT_3D('',#10012,#7832,#7833);
#6457=AXIS2_PLACEMENT_3D('',#10014,#7835,#7836);
#6458=AXIS2_PLACEMENT_3D('',#10018,#7838,#7839);
#6459=AXIS2_PLACEMENT_3D('',#10019,#7840,#7841);
#6460=AXIS2_PLACEMENT_3D('',#10073,#7843,#7844);
#6461=AXIS2_PLACEMENT_3D('',#10099,#7845,#7846);
#6462=AXIS2_PLACEMENT_3D('',#10101,#7848,#7849);
#6463=AXIS2_PLACEMENT_3D('',#10103,#7850,#7851);
#6464=AXIS2_PLACEMENT_3D('',#10107,#7854,#7855);
#6465=AXIS2_PLACEMENT_3D('',#10108,#7856,#7857);
#6466=AXIS2_PLACEMENT_3D('',#10110,#7858,#7859);
#6467=AXIS2_PLACEMENT_3D('',#10114,#7862,#7863);
#6468=AXIS2_PLACEMENT_3D('',#10115,#7864,#7865);
#6469=AXIS2_PLACEMENT_3D('',#10116,#7866,#7867);
#6470=AXIS2_PLACEMENT_3D('',#10117,#7868,#7869);
#6471=AXIS2_PLACEMENT_3D('',#10118,#7870,#7871);
#6472=AXIS2_PLACEMENT_3D('',#10120,#7872,#7873);
#6473=AXIS2_PLACEMENT_3D('',#10122,#7874,#7875);
#6474=AXIS2_PLACEMENT_3D('',#10123,#7876,#7877);
#6475=AXIS2_PLACEMENT_3D('',#10125,#7878,#7879);
#6476=AXIS2_PLACEMENT_3D('',#10127,#7880,#7881);
#6477=AXIS2_PLACEMENT_3D('',#10128,#7882,#7883);
#6478=AXIS2_PLACEMENT_3D('',#10130,#7885,#7886);
#6479=AXIS2_PLACEMENT_3D('',#10133,#7888,#7889);
#6480=AXIS2_PLACEMENT_3D('',#10134,#7890,#7891);
#6481=AXIS2_PLACEMENT_3D('',#10136,#7892,#7893);
#6482=AXIS2_PLACEMENT_3D('',#10138,#7895,#7896);
#6483=AXIS2_PLACEMENT_3D('',#10139,#7897,#7898);
#6484=AXIS2_PLACEMENT_3D('',#10140,#7899,#7900);
#6485=AXIS2_PLACEMENT_3D('',#10141,#7901,#7902);
#6486=AXIS2_PLACEMENT_3D('',#10143,#7903,#7904);
#6487=AXIS2_PLACEMENT_3D('',#10146,#7906,#7907);
#6488=AXIS2_PLACEMENT_3D('',#10147,#7908,#7909);
#6489=AXIS2_PLACEMENT_3D('',#10152,#7911,#7912);
#6490=AXIS2_PLACEMENT_3D('',#10155,#7914,#7915);
#6491=AXIS2_PLACEMENT_3D('',#10156,#7916,#7917);
#6492=AXIS2_PLACEMENT_3D('',#10160,#7919,#7920);
#6493=AXIS2_PLACEMENT_3D('',#10162,#7922,#7923);
#6494=AXIS2_PLACEMENT_3D('',#10166,#7926,#7927);
#6495=AXIS2_PLACEMENT_3D('',#10170,#7930,#7931);
#6496=AXIS2_PLACEMENT_3D('',#10171,#7932,#7933);
#6497=AXIS2_PLACEMENT_3D('',#10172,#7934,#7935);
#6498=AXIS2_PLACEMENT_3D('',#10173,#7936,#7937);
#6499=AXIS2_PLACEMENT_3D('',#10174,#7938,#7939);
#6500=AXIS2_PLACEMENT_3D('',#10176,#7940,#7941);
#6501=AXIS2_PLACEMENT_3D('',#10179,#7943,#7944);
#6502=AXIS2_PLACEMENT_3D('',#10180,#7945,#7946);
#6503=AXIS2_PLACEMENT_3D('',#10182,#7947,#7948);
#6504=AXIS2_PLACEMENT_3D('',#10185,#7950,#7951);
#6505=AXIS2_PLACEMENT_3D('',#10186,#7952,#7953);
#6506=AXIS2_PLACEMENT_3D('',#10187,#7954,#7955);
#6507=AXIS2_PLACEMENT_3D('',#10188,#7956,#7957);
#6508=AXIS2_PLACEMENT_3D('',#10189,#7958,#7959);
#6509=AXIS2_PLACEMENT_3D('',#10191,#7960,#7961);
#6510=AXIS2_PLACEMENT_3D('',#10194,#7963,#7964);
#6511=AXIS2_PLACEMENT_3D('',#10195,#7965,#7966);
#6512=AXIS2_PLACEMENT_3D('',#10197,#7967,#7968);
#6513=AXIS2_PLACEMENT_3D('',#10200,#7970,#7971);
#6514=AXIS2_PLACEMENT_3D('',#10201,#7972,#7973);
#6515=AXIS2_PLACEMENT_3D('',#10202,#7974,#7975);
#6516=AXIS2_PLACEMENT_3D('',#10203,#7976,#7977);
#6517=AXIS2_PLACEMENT_3D('',#10204,#7978,#7979);
#6518=AXIS2_PLACEMENT_3D('',#10206,#7980,#7981);
#6519=AXIS2_PLACEMENT_3D('',#10209,#7983,#7984);
#6520=AXIS2_PLACEMENT_3D('',#10210,#7985,#7986);
#6521=AXIS2_PLACEMENT_3D('',#10212,#7987,#7988);
#6522=AXIS2_PLACEMENT_3D('',#10215,#7990,#7991);
#6523=AXIS2_PLACEMENT_3D('',#10216,#7992,#7993);
#6524=AXIS2_PLACEMENT_3D('',#10217,#7994,#7995);
#6525=AXIS2_PLACEMENT_3D('',#10218,#7996,#7997);
#6526=AXIS2_PLACEMENT_3D('',#10219,#7998,#7999);
#6527=AXIS2_PLACEMENT_3D('',#10228,#8004,#8005);
#6528=AXIS2_PLACEMENT_3D('',#10234,#8009,#8010);
#6529=AXIS2_PLACEMENT_3D('',#10240,#8014,#8015);
#6530=AXIS2_PLACEMENT_3D('',#10246,#8019,#8020);
#6531=AXIS2_PLACEMENT_3D('',#10252,#8024,#8025);
#6532=AXIS2_PLACEMENT_3D('',#10255,#8028,#8029);
#6533=AXIS2_PLACEMENT_3D('',#10256,#8030,#8031);
#6534=AXIS2_PLACEMENT_3D('',#10257,#8032,#8033);
#6535=AXIS2_PLACEMENT_3D('',#10259,#8034,#8035);
#6536=AXIS2_PLACEMENT_3D('',#10260,#8036,#8037);
#6537=AXIS2_PLACEMENT_3D('',#10262,#8038,#8039);
#6538=AXIS2_PLACEMENT_3D('',#10263,#8040,#8041);
#6539=AXIS2_PLACEMENT_3D('',#10265,#8042,#8043);
#6540=AXIS2_PLACEMENT_3D('',#10267,#8045,#8046);
#6541=AXIS2_PLACEMENT_3D('',#10269,#8047,#8048);
#6542=AXIS2_PLACEMENT_3D('',#10271,#8050,#8051);
#6543=AXIS2_PLACEMENT_3D('',#10273,#8052,#8053);
#6544=AXIS2_PLACEMENT_3D('',#10275,#8055,#8056);
#6545=AXIS2_PLACEMENT_3D('',#10277,#8057,#8058);
#6546=AXIS2_PLACEMENT_3D('',#10278,#8059,#8060);
#6547=AXIS2_PLACEMENT_3D('',#10280,#8061,#8062);
#6548=AXIS2_PLACEMENT_3D('',#10282,#8064,#8065);
#6549=AXIS2_PLACEMENT_3D('',#10284,#8067,#8068);
#6550=AXIS2_PLACEMENT_3D('',#10285,#8069,#8070);
#6551=AXIS2_PLACEMENT_3D('',#10286,#8071,#8072);
#6552=AXIS2_PLACEMENT_3D('',#10287,#8073,#8074);
#6553=AXIS2_PLACEMENT_3D('',#10288,#8075,#8076);
#6554=AXIS2_PLACEMENT_3D('',#10289,#8077,#8078);
#6555=AXIS2_PLACEMENT_3D('',#10290,#8079,#8080);
#6556=AXIS2_PLACEMENT_3D('',#10291,#8081,#8082);
#6557=AXIS2_PLACEMENT_3D('',#10292,#8083,#8084);
#6558=AXIS2_PLACEMENT_3D('',#10293,#8085,#8086);
#6559=AXIS2_PLACEMENT_3D('',#10294,#8087,#8088);
#6560=AXIS2_PLACEMENT_3D('',#10295,#8089,#8090);
#6561=AXIS2_PLACEMENT_3D('',#10296,#8091,#8092);
#6562=AXIS2_PLACEMENT_3D('',#10297,#8093,#8094);
#6563=AXIS2_PLACEMENT_3D('',#10298,#8095,#8096);
#6564=AXIS2_PLACEMENT_3D('',#10299,#8097,#8098);
#6565=AXIS2_PLACEMENT_3D('',#10300,#8099,#8100);
#6566=AXIS2_PLACEMENT_3D('',#10301,#8101,#8102);
#6567=AXIS2_PLACEMENT_3D('',#10302,#8103,#8104);
#6568=AXIS2_PLACEMENT_3D('',#10303,#8105,#8106);
#6569=AXIS2_PLACEMENT_3D('',#10304,#8107,#8108);
#6570=AXIS2_PLACEMENT_3D('',#10305,#8109,#8110);
#6571=AXIS2_PLACEMENT_3D('',#10306,#8111,#8112);
#6572=AXIS2_PLACEMENT_3D('',#10308,#8113,#8114);
#6573=AXIS2_PLACEMENT_3D('',#10311,#8116,#8117);
#6574=AXIS2_PLACEMENT_3D('',#10312,#8118,#8119);
#6575=AXIS2_PLACEMENT_3D('',#10314,#8120,#8121);
#6576=AXIS2_PLACEMENT_3D('',#10317,#8123,#8124);
#6577=AXIS2_PLACEMENT_3D('',#10318,#8125,#8126);
#6578=AXIS2_PLACEMENT_3D('',#10320,#8127,#8128);
#6579=AXIS2_PLACEMENT_3D('',#10323,#8130,#8131);
#6580=AXIS2_PLACEMENT_3D('',#10324,#8132,#8133);
#6581=AXIS2_PLACEMENT_3D('',#10326,#8134,#8135);
#6582=AXIS2_PLACEMENT_3D('',#10329,#8137,#8138);
#6583=AXIS2_PLACEMENT_3D('',#10330,#8139,#8140);
#6584=AXIS2_PLACEMENT_3D('',#10333,#8141,#8142);
#6585=AXIS2_PLACEMENT_3D('',#10337,#8144,#8145);
#6586=AXIS2_PLACEMENT_3D('',#10339,#8147,#8148);
#6587=AXIS2_PLACEMENT_3D('',#10342,#8149,#8150);
#6588=AXIS2_PLACEMENT_3D('',#10346,#8152,#8153);
#6589=AXIS2_PLACEMENT_3D('',#10348,#8155,#8156);
#6590=AXIS2_PLACEMENT_3D('',#10351,#8157,#8158);
#6591=AXIS2_PLACEMENT_3D('',#10355,#8160,#8161);
#6592=AXIS2_PLACEMENT_3D('',#10357,#8163,#8164);
#6593=AXIS2_PLACEMENT_3D('',#10362,#8166,#8167);
#6594=AXIS2_PLACEMENT_3D('',#10365,#8169,#8170);
#6595=AXIS2_PLACEMENT_3D('',#10366,#8171,#8172);
#6596=AXIS2_PLACEMENT_3D('',#10368,#8173,#8174);
#6597=AXIS2_PLACEMENT_3D('',#10371,#8176,#8177);
#6598=AXIS2_PLACEMENT_3D('',#10372,#8178,#8179);
#6599=AXIS2_PLACEMENT_3D('',#10374,#8180,#8181);
#6600=AXIS2_PLACEMENT_3D('',#10377,#8183,#8184);
#6601=AXIS2_PLACEMENT_3D('',#10378,#8185,#8186);
#6602=AXIS2_PLACEMENT_3D('',#10380,#8187,#8188);
#6603=AXIS2_PLACEMENT_3D('',#10383,#8190,#8191);
#6604=AXIS2_PLACEMENT_3D('',#10384,#8192,#8193);
#6605=AXIS2_PLACEMENT_3D('',#10392,#8197,#8198);
#6606=AXIS2_PLACEMENT_3D('',#10399,#8202,#8203);
#6607=AXIS2_PLACEMENT_3D('',#10401,#8204,#8205);
#6608=AXIS2_PLACEMENT_3D('',#10409,#8209,#8210);
#6609=AXIS2_PLACEMENT_3D('',#10416,#8214,#8215);
#6610=AXIS2_PLACEMENT_3D('',#10424,#8219,#8220);
#6611=AXIS2_PLACEMENT_3D('',#10431,#8224,#8225);
#6612=AXIS2_PLACEMENT_3D('',#10439,#8229,#8230);
#6613=AXIS2_PLACEMENT_3D('',#10446,#8234,#8235);
#6614=AXIS2_PLACEMENT_3D('',#10447,#8236,#8237);
#6615=AXIS2_PLACEMENT_3D('',#10449,#8238,#8239);
#6616=AXIS2_PLACEMENT_3D('',#10451,#8241,#8242);
#6617=AXIS2_PLACEMENT_3D('',#10454,#8244,#8245);
#6618=AXIS2_PLACEMENT_3D('',#10455,#8246,#8247);
#6619=AXIS2_PLACEMENT_3D('',#10459,#8250,#8251);
#6620=AXIS2_PLACEMENT_3D('',#10463,#8254,#8255);
#6621=AXIS2_PLACEMENT_3D('',#10469,#8259,#8260);
#6622=AXIS2_PLACEMENT_3D('',#10471,#8262,#8263);
#6623=AXIS2_PLACEMENT_3D('',#10475,#8266,#8267);
#6624=AXIS2_PLACEMENT_3D('',#10477,#8268,#8269);
#6625=AXIS2_PLACEMENT_3D('',#10485,#8273,#8274);
#6626=AXIS2_PLACEMENT_3D('',#10487,#8275,#8276);
#6627=AXIS2_PLACEMENT_3D('',#10488,#8277,#8278);
#6628=AXIS2_PLACEMENT_3D('',#10489,#8279,#8280);
#6629=AXIS2_PLACEMENT_3D('',#10493,#8282,#8283);
#6630=AXIS2_PLACEMENT_3D('',#10495,#8284,#8285);
#6631=AXIS2_PLACEMENT_3D('',#10497,#8286,#8287);
#6632=AXIS2_PLACEMENT_3D('',#10503,#8291,#8292);
#6633=AXIS2_PLACEMENT_3D('',#10506,#8293,#8294);
#6634=AXIS2_PLACEMENT_3D('',#10507,#8295,#8296);
#6635=AXIS2_PLACEMENT_3D('',#10508,#8297,#8298);
#6636=AXIS2_PLACEMENT_3D('',#10512,#8302,#8303);
#6637=AXIS2_PLACEMENT_3D('',#10516,#8305,#8306);
#6638=AXIS2_PLACEMENT_3D('',#10519,#8308,#8309);
#6639=AXIS2_PLACEMENT_3D('',#10521,#8310,#8311);
#6640=AXIS2_PLACEMENT_3D('',#10525,#8313,#8314);
#6641=AXIS2_PLACEMENT_3D('',#10529,#8316,#8317);
#6642=AXIS2_PLACEMENT_3D('',#10533,#8319,#8320);
#6643=AXIS2_PLACEMENT_3D('',#10537,#8322,#8323);
#6644=AXIS2_PLACEMENT_3D('',#10539,#8325,#8326);
#6645=AXIS2_PLACEMENT_3D('',#10540,#8327,#8328);
#6646=AXIS2_PLACEMENT_3D('',#10542,#8330,#8331);
#6647=AXIS2_PLACEMENT_3D('',#10544,#8333,#8334);
#6648=AXIS2_PLACEMENT_3D('',#10546,#8336,#8337);
#6649=AXIS2_PLACEMENT_3D('',#10552,#8341,#8342);
#6650=AXIS2_PLACEMENT_3D('',#10554,#8344,#8345);
#6651=AXIS2_PLACEMENT_3D('',#10558,#8348,#8349);
#6652=AXIS2_PLACEMENT_3D('',#10560,#8350,#8351);
#6653=AXIS2_PLACEMENT_3D('',#10567,#8355,#8356);
#6654=AXIS2_PLACEMENT_3D('',#10568,#8357,#8358);
#6655=AXIS2_PLACEMENT_3D('',#10569,#8359,#8360);
#6656=AXIS2_PLACEMENT_3D('',#10570,#8361,#8362);
#6657=AXIS2_PLACEMENT_3D('',#10571,#8363,#8364);
#6658=AXIS2_PLACEMENT_3D('',#10573,#8366,#8367);
#6659=AXIS2_PLACEMENT_3D('',#10574,#8368,#8369);
#6660=AXIS2_PLACEMENT_3D('',#10576,#8371,#8372);
#6661=AXIS2_PLACEMENT_3D('',#10578,#8374,#8375);
#6662=AXIS2_PLACEMENT_3D('',#10580,#8377,#8378);
#6663=AXIS2_PLACEMENT_3D('',#10586,#8382,#8383);
#6664=AXIS2_PLACEMENT_3D('',#10588,#8385,#8386);
#6665=AXIS2_PLACEMENT_3D('',#10592,#8389,#8390);
#6666=AXIS2_PLACEMENT_3D('',#10594,#8391,#8392);
#6667=AXIS2_PLACEMENT_3D('',#10601,#8396,#8397);
#6668=AXIS2_PLACEMENT_3D('',#10602,#8398,#8399);
#6669=AXIS2_PLACEMENT_3D('',#10603,#8400,#8401);
#6670=AXIS2_PLACEMENT_3D('',#10604,#8402,#8403);
#6671=AXIS2_PLACEMENT_3D('',#10605,#8404,#8405);
#6672=AXIS2_PLACEMENT_3D('',#10607,#8407,#8408);
#6673=AXIS2_PLACEMENT_3D('',#10608,#8409,#8410);
#6674=AXIS2_PLACEMENT_3D('',#10610,#8412,#8413);
#6675=AXIS2_PLACEMENT_3D('',#10612,#8415,#8416);
#6676=AXIS2_PLACEMENT_3D('',#10614,#8418,#8419);
#6677=AXIS2_PLACEMENT_3D('',#10616,#8421,#8422);
#6678=AXIS2_PLACEMENT_3D('',#10618,#8424,#8425);
#6679=AXIS2_PLACEMENT_3D('',#10619,#8426,#8427);
#6680=AXIS2_PLACEMENT_3D('',#10620,#8428,#8429);
#6681=AXIS2_PLACEMENT_3D('',#10623,#8432,#8433);
#6682=AXIS2_PLACEMENT_3D('',#10624,#8434,#8435);
#6683=AXIS2_PLACEMENT_3D('',#10625,#8436,#8437);
#6684=AXIS2_PLACEMENT_3D('',#10627,#8438,#8439);
#6685=AXIS2_PLACEMENT_3D('',#10628,#8440,#8441);
#6686=AXIS2_PLACEMENT_3D('',#10631,#8443,#8444);
#6687=AXIS2_PLACEMENT_3D('',#10632,#8445,#8446);
#6688=AXIS2_PLACEMENT_3D('',#10633,#8447,#8448);
#6689=AXIS2_PLACEMENT_3D('',#10634,#8449,#8450);
#6690=AXIS2_PLACEMENT_3D('',#10636,#8451,#8452);
#6691=AXIS2_PLACEMENT_3D('',#10639,#8454,#8455);
#6692=AXIS2_PLACEMENT_3D('',#10640,#8456,#8457);
#6693=AXIS2_PLACEMENT_3D('',#10642,#8458,#8459);
#6694=AXIS2_PLACEMENT_3D('',#10645,#8461,#8462);
#6695=AXIS2_PLACEMENT_3D('',#10646,#8463,#8464);
#6696=AXIS2_PLACEMENT_3D('',#10647,#8465,#8466);
#6697=AXIS2_PLACEMENT_3D('',#10648,#8467,#8468);
#6698=AXIS2_PLACEMENT_3D('',#10649,#8469,#8470);
#6699=AXIS2_PLACEMENT_3D('',#10654,#8472,#8473);
#6700=AXIS2_PLACEMENT_3D('',#10655,#8474,#8475);
#6701=AXIS2_PLACEMENT_3D('',#10656,#8476,#8477);
#6702=AXIS2_PLACEMENT_3D('',#10709,#8479,#8480);
#6703=AXIS2_PLACEMENT_3D('',#10724,#8481,#8482);
#6704=AXIS2_PLACEMENT_3D('',#10726,#8484,#8485);
#6705=AXIS2_PLACEMENT_3D('',#10730,#8487,#8488);
#6706=AXIS2_PLACEMENT_3D('',#10731,#8489,#8490);
#6707=AXIS2_PLACEMENT_3D('',#10785,#8492,#8493);
#6708=AXIS2_PLACEMENT_3D('',#10811,#8494,#8495);
#6709=AXIS2_PLACEMENT_3D('',#10813,#8497,#8498);
#6710=AXIS2_PLACEMENT_3D('',#10815,#8499,#8500);
#6711=AXIS2_PLACEMENT_3D('',#10819,#8503,#8504);
#6712=AXIS2_PLACEMENT_3D('',#10820,#8505,#8506);
#6713=AXIS2_PLACEMENT_3D('',#10822,#8507,#8508);
#6714=AXIS2_PLACEMENT_3D('',#10826,#8511,#8512);
#6715=AXIS2_PLACEMENT_3D('',#10827,#8513,#8514);
#6716=AXIS2_PLACEMENT_3D('',#10828,#8515,#8516);
#6717=AXIS2_PLACEMENT_3D('',#10829,#8517,#8518);
#6718=AXIS2_PLACEMENT_3D('',#10830,#8519,#8520);
#6719=AXIS2_PLACEMENT_3D('',#10832,#8521,#8522);
#6720=AXIS2_PLACEMENT_3D('',#10833,#8523,#8524);
#6721=AXIS2_PLACEMENT_3D('',#10842,#8529,#8530);
#6722=AXIS2_PLACEMENT_3D('',#10848,#8534,#8535);
#6723=AXIS2_PLACEMENT_3D('',#10854,#8539,#8540);
#6724=AXIS2_PLACEMENT_3D('',#10860,#8544,#8545);
#6725=AXIS2_PLACEMENT_3D('',#10866,#8549,#8550);
#6726=AXIS2_PLACEMENT_3D('',#10869,#8553,#8554);
#6727=AXIS2_PLACEMENT_3D('',#10870,#8555,#8556);
#6728=AXIS2_PLACEMENT_3D('',#10872,#8557,#8558);
#6729=AXIS2_PLACEMENT_3D('',#10873,#8559,#8560);
#6730=AXIS2_PLACEMENT_3D('',#10875,#8561,#8562);
#6731=AXIS2_PLACEMENT_3D('',#10877,#8564,#8565);
#6732=AXIS2_PLACEMENT_3D('',#10879,#8567,#8568);
#6733=AXIS2_PLACEMENT_3D('',#10880,#8569,#8570);
#6734=AXIS2_PLACEMENT_3D('',#10881,#8571,#8572);
#6735=AXIS2_PLACEMENT_3D('',#10882,#8573,#8574);
#6736=AXIS2_PLACEMENT_3D('',#10883,#8575,#8576);
#6737=AXIS2_PLACEMENT_3D('',#10884,#8577,#8578);
#6738=AXIS2_PLACEMENT_3D('',#10885,#8579,#8580);
#6739=AXIS2_PLACEMENT_3D('',#10886,#8581,#8582);
#6740=AXIS2_PLACEMENT_3D('',#10887,#8583,#8584);
#6741=AXIS2_PLACEMENT_3D('',#10888,#8585,#8586);
#6742=AXIS2_PLACEMENT_3D('',#10889,#8587,#8588);
#6743=AXIS2_PLACEMENT_3D('',#10890,#8589,#8590);
#6744=AXIS2_PLACEMENT_3D('',#10891,#8591,#8592);
#6745=AXIS2_PLACEMENT_3D('',#10892,#8593,#8594);
#6746=AXIS2_PLACEMENT_3D('',#10893,#8595,#8596);
#6747=AXIS2_PLACEMENT_3D('',#10894,#8597,#8598);
#6748=AXIS2_PLACEMENT_3D('',#10895,#8599,#8600);
#6749=DIRECTION('axis',(0.,0.,1.));
#6750=DIRECTION('refdir',(1.,0.,0.));
#6751=DIRECTION('axis',(0.,0.,1.));
#6752=DIRECTION('refdir',(1.,0.,0.));
#6753=DIRECTION('axis',(0.,0.,1.));
#6754=DIRECTION('refdir',(1.,0.,0.));
#6755=DIRECTION('center_axis',(0.,0.,1.));
#6756=DIRECTION('ref_axis',(1.,0.,0.));
#6757=DIRECTION('center_axis',(0.,0.,1.));
#6758=DIRECTION('ref_axis',(1.,0.,0.));
#6759=DIRECTION('',(0.,0.,1.));
#6760=DIRECTION('center_axis',(0.,0.,-1.));
#6761=DIRECTION('ref_axis',(1.,0.,0.));
#6762=DIRECTION('center_axis',(0.,0.,1.));
#6763=DIRECTION('ref_axis',(1.,0.,0.));
#6764=DIRECTION('center_axis',(0.,0.,1.));
#6765=DIRECTION('ref_axis',(1.,0.,0.));
#6766=DIRECTION('',(0.,0.,1.));
#6767=DIRECTION('center_axis',(0.,0.,-1.));
#6768=DIRECTION('ref_axis',(1.,0.,0.));
#6769=DIRECTION('center_axis',(0.,0.,1.));
#6770=DIRECTION('ref_axis',(1.,0.,0.));
#6771=DIRECTION('center_axis',(0.,0.,1.));
#6772=DIRECTION('ref_axis',(1.,0.,0.));
#6773=DIRECTION('',(0.,0.,1.));
#6774=DIRECTION('center_axis',(0.,0.,-1.));
#6775=DIRECTION('ref_axis',(1.,0.,0.));
#6776=DIRECTION('center_axis',(0.,0.,1.));
#6777=DIRECTION('ref_axis',(1.,0.,0.));
#6778=DIRECTION('center_axis',(0.,0.,1.));
#6779=DIRECTION('ref_axis',(1.,0.,0.));
#6780=DIRECTION('',(0.,0.,1.));
#6781=DIRECTION('center_axis',(0.,0.,-1.));
#6782=DIRECTION('ref_axis',(1.,0.,0.));
#6783=DIRECTION('center_axis',(0.,1.,0.));
#6784=DIRECTION('ref_axis',(-1.,0.,0.));
#6785=DIRECTION('',(-1.,0.,0.));
#6786=DIRECTION('',(0.,0.,1.));
#6787=DIRECTION('',(-1.,0.,0.));
#6788=DIRECTION('',(0.,0.,1.));
#6789=DIRECTION('center_axis',(1.,0.,0.));
#6790=DIRECTION('ref_axis',(0.,1.,0.));
#6791=DIRECTION('',(0.,1.,0.));
#6792=DIRECTION('',(0.,1.,0.));
#6793=DIRECTION('',(0.,0.,1.));
#6794=DIRECTION('center_axis',(0.,-1.,0.));
#6795=DIRECTION('ref_axis',(1.,0.,0.));
#6796=DIRECTION('',(1.,0.,0.));
#6797=DIRECTION('',(1.,0.,0.));
#6798=DIRECTION('',(0.,0.,1.));
#6799=DIRECTION('center_axis',(-1.,0.,0.));
#6800=DIRECTION('ref_axis',(0.,-1.,0.));
#6801=DIRECTION('',(0.,-1.,0.));
#6802=DIRECTION('',(0.,-1.,0.));
#6803=DIRECTION('center_axis',(0.,0.,1.));
#6804=DIRECTION('ref_axis',(1.,0.,0.));
#6805=DIRECTION('center_axis',(0.,0.,1.));
#6806=DIRECTION('ref_axis',(1.,0.,0.));
#6807=DIRECTION('axis',(0.,0.,1.));
#6808=DIRECTION('refdir',(1.,0.,0.));
#6809=DIRECTION('center_axis',(0.,1.,0.));
#6810=DIRECTION('ref_axis',(-1.,0.,0.));
#6811=DIRECTION('',(-1.,0.,0.));
#6812=DIRECTION('',(0.,0.,1.));
#6813=DIRECTION('',(-1.,0.,0.));
#6814=DIRECTION('',(0.,0.,1.));
#6815=DIRECTION('center_axis',(1.,0.,0.));
#6816=DIRECTION('ref_axis',(0.,1.,0.));
#6817=DIRECTION('',(0.,1.,0.));
#6818=DIRECTION('',(0.,1.,0.));
#6819=DIRECTION('',(0.,0.,1.));
#6820=DIRECTION('center_axis',(0.,-1.,0.));
#6821=DIRECTION('ref_axis',(1.,0.,0.));
#6822=DIRECTION('',(1.,0.,0.));
#6823=DIRECTION('',(1.,0.,0.));
#6824=DIRECTION('',(0.,0.,1.));
#6825=DIRECTION('center_axis',(-1.,0.,0.));
#6826=DIRECTION('ref_axis',(0.,-1.,0.));
#6827=DIRECTION('',(0.,-1.,0.));
#6828=DIRECTION('',(0.,-1.,0.));
#6829=DIRECTION('center_axis',(0.,0.,1.));
#6830=DIRECTION('ref_axis',(1.,0.,0.));
#6831=DIRECTION('center_axis',(0.,0.,1.));
#6832=DIRECTION('ref_axis',(1.,0.,0.));
#6833=DIRECTION('axis',(0.,0.,1.));
#6834=DIRECTION('refdir',(1.,0.,0.));
#6835=DIRECTION('center_axis',(0.,1.,0.));
#6836=DIRECTION('ref_axis',(-1.,0.,0.));
#6837=DIRECTION('',(-1.,0.,0.));
#6838=DIRECTION('',(0.,0.,1.));
#6839=DIRECTION('',(-1.,0.,0.));
#6840=DIRECTION('',(0.,0.,1.));
#6841=DIRECTION('center_axis',(1.,0.,0.));
#6842=DIRECTION('ref_axis',(0.,1.,0.));
#6843=DIRECTION('',(0.,1.,0.));
#6844=DIRECTION('',(0.,1.,0.));
#6845=DIRECTION('',(0.,0.,1.));
#6846=DIRECTION('center_axis',(0.,-1.,0.));
#6847=DIRECTION('ref_axis',(1.,0.,0.));
#6848=DIRECTION('',(1.,0.,0.));
#6849=DIRECTION('',(1.,0.,0.));
#6850=DIRECTION('',(0.,0.,1.));
#6851=DIRECTION('center_axis',(-1.,0.,0.));
#6852=DIRECTION('ref_axis',(0.,-1.,0.));
#6853=DIRECTION('',(0.,-1.,0.));
#6854=DIRECTION('',(0.,-1.,0.));
#6855=DIRECTION('center_axis',(0.,0.,1.));
#6856=DIRECTION('ref_axis',(1.,0.,0.));
#6857=DIRECTION('center_axis',(0.,0.,1.));
#6858=DIRECTION('ref_axis',(1.,0.,0.));
#6859=DIRECTION('axis',(0.,0.,1.));
#6860=DIRECTION('refdir',(1.,0.,0.));
#6861=DIRECTION('center_axis',(0.,1.,0.));
#6862=DIRECTION('ref_axis',(1.,0.,0.));
#6863=DIRECTION('center_axis',(0.,1.,0.));
#6864=DIRECTION('ref_axis',(1.,0.,0.));
#6865=DIRECTION('',(0.,1.,0.));
#6866=DIRECTION('center_axis',(0.,0.,1.));
#6867=DIRECTION('ref_axis',(1.,0.,0.));
#6868=DIRECTION('center_axis',(0.,0.,1.));
#6869=DIRECTION('ref_axis',(1.,0.,0.));
#6870=DIRECTION('',(0.,0.,1.));
#6871=DIRECTION('center_axis',(0.,0.,-1.));
#6872=DIRECTION('ref_axis',(1.,0.,0.));
#6873=DIRECTION('center_axis',(0.,0.,1.));
#6874=DIRECTION('ref_axis',(1.,0.,0.));
#6875=DIRECTION('center_axis',(0.,0.,1.));
#6876=DIRECTION('ref_axis',(1.,0.,0.));
#6877=DIRECTION('center_axis',(0.,0.,1.));
#6878=DIRECTION('ref_axis',(1.,0.,0.));
#6879=DIRECTION('',(0.,0.,1.));
#6880=DIRECTION('center_axis',(0.,0.,-1.));
#6881=DIRECTION('ref_axis',(1.,0.,0.));
#6882=DIRECTION('center_axis',(0.,0.,1.));
#6883=DIRECTION('ref_axis',(1.,0.,0.));
#6884=DIRECTION('center_axis',(0.,0.,1.));
#6885=DIRECTION('ref_axis',(1.,0.,0.));
#6886=DIRECTION('center_axis',(0.,0.,1.));
#6887=DIRECTION('ref_axis',(1.,0.,0.));
#6888=DIRECTION('',(0.,0.,1.));
#6889=DIRECTION('center_axis',(0.,0.,-1.));
#6890=DIRECTION('ref_axis',(1.,0.,0.));
#6891=DIRECTION('center_axis',(0.,0.,1.));
#6892=DIRECTION('ref_axis',(1.,0.,0.));
#6893=DIRECTION('center_axis',(0.,0.,1.));
#6894=DIRECTION('ref_axis',(1.,0.,0.));
#6895=DIRECTION('center_axis',(0.,0.,1.));
#6896=DIRECTION('ref_axis',(1.,0.,0.));
#6897=DIRECTION('',(0.,0.,1.));
#6898=DIRECTION('center_axis',(0.,0.,-1.));
#6899=DIRECTION('ref_axis',(1.,0.,0.));
#6900=DIRECTION('center_axis',(0.,0.,1.));
#6901=DIRECTION('ref_axis',(1.,0.,0.));
#6902=DIRECTION('center_axis',(0.,0.,1.));
#6903=DIRECTION('ref_axis',(1.,0.,0.));
#6904=DIRECTION('center_axis',(0.,0.,1.));
#6905=DIRECTION('ref_axis',(1.,0.,0.));
#6906=DIRECTION('',(0.,0.,1.));
#6907=DIRECTION('center_axis',(0.,0.,-1.));
#6908=DIRECTION('ref_axis',(1.,0.,0.));
#6909=DIRECTION('center_axis',(0.,0.,1.));
#6910=DIRECTION('ref_axis',(1.,0.,0.));
#6911=DIRECTION('center_axis',(0.,0.,1.));
#6912=DIRECTION('ref_axis',(1.,0.,0.));
#6913=DIRECTION('center_axis',(0.,0.,1.));
#6914=DIRECTION('ref_axis',(1.,0.,0.));
#6915=DIRECTION('center_axis',(0.,0.,1.));
#6916=DIRECTION('ref_axis',(1.,0.,0.));
#6917=DIRECTION('',(0.,0.,1.));
#6918=DIRECTION('center_axis',(0.,1.,0.));
#6919=DIRECTION('ref_axis',(1.,0.,0.));
#6920=DIRECTION('center_axis',(0.,1.,0.));
#6921=DIRECTION('ref_axis',(1.,0.,0.));
#6922=DIRECTION('',(0.,1.,0.));
#6923=DIRECTION('center_axis',(0.,0.,1.));
#6924=DIRECTION('ref_axis',(1.,0.,0.));
#6925=DIRECTION('center_axis',(0.,0.,1.));
#6926=DIRECTION('ref_axis',(1.,0.,0.));
#6927=DIRECTION('',(0.,0.,1.));
#6928=DIRECTION('center_axis',(0.,0.,-1.));
#6929=DIRECTION('ref_axis',(1.,0.,0.));
#6930=DIRECTION('center_axis',(0.,0.,1.));
#6931=DIRECTION('ref_axis',(1.,0.,0.));
#6932=DIRECTION('center_axis',(0.,0.,1.));
#6933=DIRECTION('ref_axis',(1.,0.,0.));
#6934=DIRECTION('center_axis',(0.,0.,1.));
#6935=DIRECTION('ref_axis',(1.,0.,0.));
#6936=DIRECTION('',(0.,0.,1.));
#6937=DIRECTION('center_axis',(0.,0.,-1.));
#6938=DIRECTION('ref_axis',(1.,0.,0.));
#6939=DIRECTION('center_axis',(0.,0.,1.));
#6940=DIRECTION('ref_axis',(1.,0.,0.));
#6941=DIRECTION('center_axis',(0.,0.,1.));
#6942=DIRECTION('ref_axis',(1.,0.,0.));
#6943=DIRECTION('center_axis',(0.,0.,1.));
#6944=DIRECTION('ref_axis',(1.,0.,0.));
#6945=DIRECTION('',(0.,0.,1.));
#6946=DIRECTION('center_axis',(0.,0.,-1.));
#6947=DIRECTION('ref_axis',(1.,0.,0.));
#6948=DIRECTION('center_axis',(0.,0.,1.));
#6949=DIRECTION('ref_axis',(1.,0.,0.));
#6950=DIRECTION('center_axis',(0.,0.,1.));
#6951=DIRECTION('ref_axis',(1.,0.,0.));
#6952=DIRECTION('center_axis',(0.,0.,1.));
#6953=DIRECTION('ref_axis',(1.,0.,0.));
#6954=DIRECTION('',(0.,0.,1.));
#6955=DIRECTION('center_axis',(0.,0.,-1.));
#6956=DIRECTION('ref_axis',(1.,0.,0.));
#6957=DIRECTION('center_axis',(0.,0.,1.));
#6958=DIRECTION('ref_axis',(1.,0.,0.));
#6959=DIRECTION('center_axis',(0.,0.,1.));
#6960=DIRECTION('ref_axis',(1.,0.,0.));
#6961=DIRECTION('center_axis',(0.,0.,1.));
#6962=DIRECTION('ref_axis',(1.,0.,0.));
#6963=DIRECTION('',(0.,0.,1.));
#6964=DIRECTION('center_axis',(0.,0.,-1.));
#6965=DIRECTION('ref_axis',(1.,0.,0.));
#6966=DIRECTION('center_axis',(0.,0.,1.));
#6967=DIRECTION('ref_axis',(1.,0.,0.));
#6968=DIRECTION('center_axis',(0.,0.,1.));
#6969=DIRECTION('ref_axis',(1.,0.,0.));
#6970=DIRECTION('center_axis',(0.,0.,1.));
#6971=DIRECTION('ref_axis',(1.,0.,0.));
#6972=DIRECTION('center_axis',(0.,0.,1.));
#6973=DIRECTION('ref_axis',(1.,0.,0.));
#6974=DIRECTION('',(0.,0.,1.));
#6975=DIRECTION('center_axis',(0.,0.,1.));
#6976=DIRECTION('ref_axis',(-0.707106781186547,0.707106781186548,0.));
#6977=DIRECTION('',(0.,0.,1.));
#6978=DIRECTION('center_axis',(0.,0.,-1.));
#6979=DIRECTION('ref_axis',(1.,0.,0.));
#6980=DIRECTION('',(0.,0.,1.));
#6981=DIRECTION('center_axis',(0.,0.,1.));
#6982=DIRECTION('ref_axis',(1.,0.,0.));
#6983=DIRECTION('center_axis',(0.,0.,1.));
#6984=DIRECTION('ref_axis',(1.,0.,0.));
#6985=DIRECTION('',(0.,0.,1.));
#6986=DIRECTION('center_axis',(0.,0.,1.));
#6987=DIRECTION('ref_axis',(1.,0.,0.));
#6988=DIRECTION('',(0.,0.,1.));
#6989=DIRECTION('center_axis',(0.,0.,-1.));
#6990=DIRECTION('ref_axis',(1.,0.,0.));
#6991=DIRECTION('center_axis',(0.,0.,1.));
#6992=DIRECTION('ref_axis',(1.,0.,0.));
#6993=DIRECTION('center_axis',(0.,0.,1.));
#6994=DIRECTION('ref_axis',(1.,0.,0.));
#6995=DIRECTION('center_axis',(0.,0.,1.));
#6996=DIRECTION('ref_axis',(1.,0.,0.));
#6997=DIRECTION('',(0.,0.,1.));
#6998=DIRECTION('center_axis',(0.,0.,-1.));
#6999=DIRECTION('ref_axis',(1.,0.,0.));
#7000=DIRECTION('',(0.,0.,1.));
#7001=DIRECTION('center_axis',(0.,0.,1.));
#7002=DIRECTION('ref_axis',(1.,0.,0.));
#7003=DIRECTION('center_axis',(0.,0.,1.));
#7004=DIRECTION('ref_axis',(1.,0.,0.));
#7005=DIRECTION('',(0.,0.,1.));
#7006=DIRECTION('center_axis',(0.,0.,1.));
#7007=DIRECTION('ref_axis',(1.,0.,0.));
#7008=DIRECTION('',(0.,0.,1.));
#7009=DIRECTION('center_axis',(0.,0.,-1.));
#7010=DIRECTION('ref_axis',(1.,0.,0.));
#7011=DIRECTION('center_axis',(0.,0.,1.));
#7012=DIRECTION('ref_axis',(1.,0.,0.));
#7013=DIRECTION('center_axis',(0.,0.,1.));
#7014=DIRECTION('ref_axis',(1.,0.,0.));
#7015=DIRECTION('center_axis',(0.,0.,1.));
#7016=DIRECTION('ref_axis',(1.,0.,0.));
#7017=DIRECTION('',(0.,0.,1.));
#7018=DIRECTION('center_axis',(0.,0.,-1.));
#7019=DIRECTION('ref_axis',(1.,0.,0.));
#7020=DIRECTION('',(0.,0.,1.));
#7021=DIRECTION('center_axis',(0.,0.,1.));
#7022=DIRECTION('ref_axis',(1.,0.,0.));
#7023=DIRECTION('center_axis',(0.,0.,1.));
#7024=DIRECTION('ref_axis',(1.,0.,0.));
#7025=DIRECTION('',(0.,0.,1.));
#7026=DIRECTION('center_axis',(0.,0.,1.));
#7027=DIRECTION('ref_axis',(1.,0.,0.));
#7028=DIRECTION('',(0.,0.,1.));
#7029=DIRECTION('center_axis',(0.,0.,-1.));
#7030=DIRECTION('ref_axis',(1.,0.,0.));
#7031=DIRECTION('center_axis',(0.,0.,1.));
#7032=DIRECTION('ref_axis',(1.,0.,0.));
#7033=DIRECTION('center_axis',(0.,0.,1.));
#7034=DIRECTION('ref_axis',(1.,0.,0.));
#7035=DIRECTION('center_axis',(0.,0.,1.));
#7036=DIRECTION('ref_axis',(-0.707106781186548,-0.707106781186547,0.));
#7037=DIRECTION('',(0.,0.,1.));
#7038=DIRECTION('center_axis',(0.,0.,-1.));
#7039=DIRECTION('ref_axis',(1.,0.,0.));
#7040=DIRECTION('',(0.,0.,1.));
#7041=DIRECTION('center_axis',(0.,0.,1.));
#7042=DIRECTION('ref_axis',(1.,0.,0.));
#7043=DIRECTION('center_axis',(0.,0.,1.));
#7044=DIRECTION('ref_axis',(1.,0.,0.));
#7045=DIRECTION('',(0.,0.,1.));
#7046=DIRECTION('center_axis',(0.,0.,1.));
#7047=DIRECTION('ref_axis',(1.,0.,0.));
#7048=DIRECTION('',(0.,0.,1.));
#7049=DIRECTION('center_axis',(0.,0.,-1.));
#7050=DIRECTION('ref_axis',(1.,0.,0.));
#7051=DIRECTION('center_axis',(0.,0.,1.));
#7052=DIRECTION('ref_axis',(1.,0.,0.));
#7053=DIRECTION('center_axis',(0.,0.,1.));
#7054=DIRECTION('ref_axis',(1.,0.,0.));
#7055=DIRECTION('center_axis',(0.,0.,1.));
#7056=DIRECTION('ref_axis',(1.,0.,0.));
#7057=DIRECTION('',(0.,1.,0.));
#7058=DIRECTION('',(-1.,0.,0.));
#7059=DIRECTION('center_axis',(0.,0.,1.));
#7060=DIRECTION('ref_axis',(1.,0.,0.));
#7061=DIRECTION('',(0.,-1.,0.));
#7062=DIRECTION('',(1.,0.,0.));
#7063=DIRECTION('center_axis',(0.,0.,1.));
#7064=DIRECTION('ref_axis',(1.,0.,0.));
#7065=DIRECTION('',(-1.,0.,0.));
#7066=DIRECTION('',(0.,-1.,0.));
#7067=DIRECTION('center_axis',(0.,0.,1.));
#7068=DIRECTION('ref_axis',(1.,0.,0.));
#7069=DIRECTION('',(0.,1.,0.));
#7070=DIRECTION('',(-1.,0.,0.));
#7071=DIRECTION('',(0.,-1.,0.));
#7072=DIRECTION('',(1.,0.,0.));
#7073=DIRECTION('center_axis',(0.,0.,1.));
#7074=DIRECTION('ref_axis',(1.,0.,0.));
#7075=DIRECTION('',(1.,0.,0.));
#7076=DIRECTION('',(0.,1.,0.));
#7077=DIRECTION('center_axis',(0.,0.,1.));
#7078=DIRECTION('ref_axis',(1.,0.,0.));
#7079=DIRECTION('center_axis',(0.,0.,1.));
#7080=DIRECTION('ref_axis',(1.,0.,0.));
#7081=DIRECTION('',(0.,0.,1.));
#7082=DIRECTION('center_axis',(0.,0.,1.));
#7083=DIRECTION('ref_axis',(1.,0.,0.));
#7084=DIRECTION('center_axis',(0.,0.,1.));
#7085=DIRECTION('ref_axis',(1.,0.,0.));
#7086=DIRECTION('',(0.,0.,1.));
#7087=DIRECTION('center_axis',(0.,0.,1.));
#7088=DIRECTION('ref_axis',(1.,0.,0.));
#7089=DIRECTION('center_axis',(0.,0.,1.));
#7090=DIRECTION('ref_axis',(1.,0.,0.));
#7091=DIRECTION('',(0.,0.,1.));
#7092=DIRECTION('center_axis',(0.,0.,1.));
#7093=DIRECTION('ref_axis',(1.,0.,0.));
#7094=DIRECTION('center_axis',(0.,0.,1.));
#7095=DIRECTION('ref_axis',(1.,0.,0.));
#7096=DIRECTION('',(0.,0.,1.));
#7097=DIRECTION('center_axis',(0.,1.,0.));
#7098=DIRECTION('ref_axis',(-1.,0.,0.));
#7099=DIRECTION('',(-1.,0.,0.));
#7100=DIRECTION('',(0.,0.,1.));
#7101=DIRECTION('',(0.,0.,1.));
#7102=DIRECTION('center_axis',(1.,0.,0.));
#7103=DIRECTION('ref_axis',(0.,1.,0.));
#7104=DIRECTION('',(0.,1.,0.));
#7105=DIRECTION('',(0.,0.,1.));
#7106=DIRECTION('center_axis',(0.,-1.,0.));
#7107=DIRECTION('ref_axis',(1.,0.,0.));
#7108=DIRECTION('',(1.,0.,0.));
#7109=DIRECTION('',(0.,0.,1.));
#7110=DIRECTION('center_axis',(-1.,0.,0.));
#7111=DIRECTION('ref_axis',(0.,-1.,0.));
#7112=DIRECTION('',(0.,-1.,0.));
#7113=DIRECTION('center_axis',(0.,0.,1.));
#7114=DIRECTION('ref_axis',(1.,0.,0.));
#7115=DIRECTION('axis',(0.,0.,1.));
#7116=DIRECTION('refdir',(1.,0.,0.));
#7117=DIRECTION('center_axis',(0.,0.,1.));
#7118=DIRECTION('ref_axis',(1.,0.,0.));
#7119=DIRECTION('',(0.,0.,1.));
#7120=DIRECTION('center_axis',(0.,0.,1.));
#7121=DIRECTION('ref_axis',(1.,0.,0.));
#7122=DIRECTION('',(0.,0.,-1.));
#7123=DIRECTION('center_axis',(0.,0.,-1.));
#7124=DIRECTION('ref_axis',(1.,0.,0.));
#7125=DIRECTION('center_axis',(0.,0.,1.));
#7126=DIRECTION('ref_axis',(1.,0.,0.));
#7127=DIRECTION('center_axis',(0.,0.,-1.));
#7128=DIRECTION('ref_axis',(1.,0.,0.));
#7129=DIRECTION('center_axis',(0.,0.,-1.));
#7130=DIRECTION('ref_axis',(1.,0.,0.));
#7131=DIRECTION('center_axis',(0.,0.,1.));
#7132=DIRECTION('ref_axis',(1.,0.,0.));
#7133=DIRECTION('center_axis',(0.,0.,1.));
#7134=DIRECTION('ref_axis',(1.,0.,0.));
#7135=DIRECTION('center_axis',(0.,0.,-1.));
#7136=DIRECTION('ref_axis',(1.,0.,0.));
#7137=DIRECTION('center_axis',(0.,0.,1.));
#7138=DIRECTION('ref_axis',(1.,0.,0.));
#7139=DIRECTION('center_axis',(0.,0.,1.));
#7140=DIRECTION('ref_axis',(1.,0.,0.));
#7141=DIRECTION('center_axis',(0.,0.,1.));
#7142=DIRECTION('ref_axis',(-1.83697019872103E-16,-1.,0.));
#7143=DIRECTION('',(0.,0.,-1.));
#7144=DIRECTION('center_axis',(0.,0.,-1.));
#7145=DIRECTION('ref_axis',(1.,0.,0.));
#7146=DIRECTION('',(0.,0.,1.));
#7147=DIRECTION('center_axis',(0.,0.,1.));
#7148=DIRECTION('ref_axis',(1.,0.,0.));
#7149=DIRECTION('center_axis',(0.,0.,-1.));
#7150=DIRECTION('ref_axis',(1.,0.,0.));
#7151=DIRECTION('center_axis',(0.,0.,1.));
#7152=DIRECTION('ref_axis',(1.,0.,0.));
#7153=DIRECTION('center_axis',(0.,0.,1.));
#7154=DIRECTION('ref_axis',(1.,0.,0.));
#7155=DIRECTION('center_axis',(0.,0.,1.));
#7156=DIRECTION('ref_axis',(-1.,1.22464679914735E-16,0.));
#7157=DIRECTION('',(0.,0.,-1.));
#7158=DIRECTION('center_axis',(0.,0.,-1.));
#7159=DIRECTION('ref_axis',(1.,0.,0.));
#7160=DIRECTION('',(0.,0.,1.));
#7161=DIRECTION('center_axis',(0.,0.,1.));
#7162=DIRECTION('ref_axis',(1.,0.,0.));
#7163=DIRECTION('center_axis',(0.,0.,-1.));
#7164=DIRECTION('ref_axis',(1.,0.,0.));
#7165=DIRECTION('center_axis',(0.,0.,1.));
#7166=DIRECTION('ref_axis',(1.,0.,0.));
#7167=DIRECTION('center_axis',(0.,0.,1.));
#7168=DIRECTION('ref_axis',(1.,0.,0.));
#7169=DIRECTION('center_axis',(0.,0.,1.));
#7170=DIRECTION('ref_axis',(6.12323399573677E-17,1.,0.));
#7171=DIRECTION('',(0.,0.,-1.));
#7172=DIRECTION('center_axis',(0.,0.,-1.));
#7173=DIRECTION('ref_axis',(1.,0.,0.));
#7174=DIRECTION('',(0.,0.,1.));
#7175=DIRECTION('center_axis',(0.,0.,1.));
#7176=DIRECTION('ref_axis',(1.,0.,0.));
#7177=DIRECTION('center_axis',(0.,0.,1.));
#7178=DIRECTION('ref_axis',(1.,0.,0.));
#7179=DIRECTION('center_axis',(0.,0.,1.));
#7180=DIRECTION('ref_axis',(1.,0.,0.));
#7181=DIRECTION('center_axis',(0.,0.,1.));
#7182=DIRECTION('ref_axis',(1.,0.,0.));
#7183=DIRECTION('center_axis',(0.,0.,1.));
#7184=DIRECTION('ref_axis',(1.,0.,0.));
#7185=DIRECTION('center_axis',(0.,0.,-1.));
#7186=DIRECTION('ref_axis',(1.,0.,0.));
#7187=DIRECTION('center_axis',(0.,0.,1.));
#7188=DIRECTION('ref_axis',(1.,0.,0.));
#7189=DIRECTION('center_axis',(0.,0.,1.));
#7190=DIRECTION('ref_axis',(1.,0.,0.));
#7191=DIRECTION('',(0.,0.,1.));
#7192=DIRECTION('center_axis',(0.,0.,1.));
#7193=DIRECTION('ref_axis',(1.,0.,0.));
#7194=DIRECTION('center_axis',(0.,0.,1.));
#7195=DIRECTION('ref_axis',(1.,0.,0.));
#7196=DIRECTION('',(0.,0.,1.));
#7197=DIRECTION('center_axis',(0.,0.,1.));
#7198=DIRECTION('ref_axis',(1.,0.,0.));
#7199=DIRECTION('center_axis',(0.,0.,1.));
#7200=DIRECTION('ref_axis',(1.,0.,0.));
#7201=DIRECTION('',(0.,0.,1.));
#7202=DIRECTION('center_axis',(0.,0.,1.));
#7203=DIRECTION('ref_axis',(1.,0.,0.));
#7204=DIRECTION('center_axis',(0.,0.,1.));
#7205=DIRECTION('ref_axis',(1.,0.,0.));
#7206=DIRECTION('',(0.,0.,1.));
#7207=DIRECTION('center_axis',(0.,0.,1.));
#7208=DIRECTION('ref_axis',(1.,0.,0.));
#7209=DIRECTION('center_axis',(0.,0.,1.));
#7210=DIRECTION('ref_axis',(1.,0.,0.));
#7211=DIRECTION('',(0.,0.,-1.));
#7212=DIRECTION('center_axis',(0.,0.,1.));
#7213=DIRECTION('ref_axis',(1.,0.,0.));
#7214=DIRECTION('center_axis',(0.,0.,1.));
#7215=DIRECTION('ref_axis',(1.,0.,0.));
#7216=DIRECTION('center_axis',(0.,0.,-1.));
#7217=DIRECTION('ref_axis',(1.,0.,0.));
#7218=DIRECTION('center_axis',(0.,0.,1.));
#7219=DIRECTION('ref_axis',(1.,0.,0.));
#7220=DIRECTION('',(0.,0.,-1.));
#7221=DIRECTION('center_axis',(0.,0.,1.));
#7222=DIRECTION('ref_axis',(1.,0.,0.));
#7223=DIRECTION('',(0.,0.,-1.));
#7224=DIRECTION('center_axis',(0.,0.,1.));
#7225=DIRECTION('ref_axis',(1.,0.,0.));
#7226=DIRECTION('center_axis',(0.,0.,1.));
#7227=DIRECTION('ref_axis',(1.,0.,0.));
#7228=DIRECTION('axis',(0.,0.,1.));
#7229=DIRECTION('refdir',(1.,0.,0.));
#7230=DIRECTION('center_axis',(0.,0.,1.));
#7231=DIRECTION('ref_axis',(1.,0.,0.));
#7232=DIRECTION('',(0.,0.,1.));
#7233=DIRECTION('center_axis',(0.,0.,1.));
#7234=DIRECTION('ref_axis',(1.,0.,0.));
#7235=DIRECTION('',(0.,0.,-1.));
#7236=DIRECTION('center_axis',(0.,0.,-1.));
#7237=DIRECTION('ref_axis',(1.,0.,0.));
#7238=DIRECTION('center_axis',(0.,0.,1.));
#7239=DIRECTION('ref_axis',(1.,0.,0.));
#7240=DIRECTION('center_axis',(0.,0.,-1.));
#7241=DIRECTION('ref_axis',(1.,0.,0.));
#7242=DIRECTION('center_axis',(0.,0.,-1.));
#7243=DIRECTION('ref_axis',(1.,0.,0.));
#7244=DIRECTION('center_axis',(0.,0.,1.));
#7245=DIRECTION('ref_axis',(1.,0.,0.));
#7246=DIRECTION('center_axis',(0.,0.,1.));
#7247=DIRECTION('ref_axis',(1.,0.,0.));
#7248=DIRECTION('center_axis',(0.,0.,-1.));
#7249=DIRECTION('ref_axis',(1.,0.,0.));
#7250=DIRECTION('center_axis',(0.,0.,1.));
#7251=DIRECTION('ref_axis',(1.,0.,0.));
#7252=DIRECTION('center_axis',(0.,0.,1.));
#7253=DIRECTION('ref_axis',(1.,0.,0.));
#7254=DIRECTION('center_axis',(0.,0.,1.));
#7255=DIRECTION('ref_axis',(-1.83697019872103E-16,-1.,0.));
#7256=DIRECTION('',(0.,0.,-1.));
#7257=DIRECTION('center_axis',(0.,0.,-1.));
#7258=DIRECTION('ref_axis',(1.,0.,0.));
#7259=DIRECTION('',(0.,0.,1.));
#7260=DIRECTION('center_axis',(0.,0.,1.));
#7261=DIRECTION('ref_axis',(1.,0.,0.));
#7262=DIRECTION('center_axis',(0.,0.,-1.));
#7263=DIRECTION('ref_axis',(1.,0.,0.));
#7264=DIRECTION('center_axis',(0.,0.,1.));
#7265=DIRECTION('ref_axis',(1.,0.,0.));
#7266=DIRECTION('center_axis',(0.,0.,1.));
#7267=DIRECTION('ref_axis',(1.,0.,0.));
#7268=DIRECTION('center_axis',(0.,0.,1.));
#7269=DIRECTION('ref_axis',(-1.,1.22464679914735E-16,0.));
#7270=DIRECTION('',(0.,0.,-1.));
#7271=DIRECTION('center_axis',(0.,0.,-1.));
#7272=DIRECTION('ref_axis',(1.,0.,0.));
#7273=DIRECTION('',(0.,0.,1.));
#7274=DIRECTION('center_axis',(0.,0.,1.));
#7275=DIRECTION('ref_axis',(1.,0.,0.));
#7276=DIRECTION('center_axis',(0.,0.,-1.));
#7277=DIRECTION('ref_axis',(1.,0.,0.));
#7278=DIRECTION('center_axis',(0.,0.,1.));
#7279=DIRECTION('ref_axis',(1.,0.,0.));
#7280=DIRECTION('center_axis',(0.,0.,1.));
#7281=DIRECTION('ref_axis',(1.,0.,0.));
#7282=DIRECTION('center_axis',(0.,0.,1.));
#7283=DIRECTION('ref_axis',(-6.04901474817726E-16,1.,0.));
#7284=DIRECTION('',(0.,0.,-1.));
#7285=DIRECTION('center_axis',(0.,0.,-1.));
#7286=DIRECTION('ref_axis',(1.,0.,0.));
#7287=DIRECTION('',(0.,0.,1.));
#7288=DIRECTION('center_axis',(0.,0.,1.));
#7289=DIRECTION('ref_axis',(1.,0.,0.));
#7290=DIRECTION('center_axis',(0.,0.,1.));
#7291=DIRECTION('ref_axis',(1.,0.,0.));
#7292=DIRECTION('center_axis',(0.,0.,1.));
#7293=DIRECTION('ref_axis',(1.,0.,0.));
#7294=DIRECTION('center_axis',(0.,0.,1.));
#7295=DIRECTION('ref_axis',(1.,0.,0.));
#7296=DIRECTION('center_axis',(0.,0.,1.));
#7297=DIRECTION('ref_axis',(1.,0.,0.));
#7298=DIRECTION('center_axis',(0.,0.,-1.));
#7299=DIRECTION('ref_axis',(1.,0.,0.));
#7300=DIRECTION('center_axis',(0.,0.,1.));
#7301=DIRECTION('ref_axis',(1.,0.,0.));
#7302=DIRECTION('center_axis',(0.,0.,1.));
#7303=DIRECTION('ref_axis',(1.,0.,0.));
#7304=DIRECTION('',(0.,0.,1.));
#7305=DIRECTION('center_axis',(0.,0.,1.));
#7306=DIRECTION('ref_axis',(1.,0.,0.));
#7307=DIRECTION('center_axis',(0.,0.,1.));
#7308=DIRECTION('ref_axis',(1.,0.,0.));
#7309=DIRECTION('',(0.,0.,1.));
#7310=DIRECTION('center_axis',(0.,0.,1.));
#7311=DIRECTION('ref_axis',(1.,0.,0.));
#7312=DIRECTION('center_axis',(0.,0.,1.));
#7313=DIRECTION('ref_axis',(1.,0.,0.));
#7314=DIRECTION('',(0.,0.,1.));
#7315=DIRECTION('center_axis',(0.,0.,1.));
#7316=DIRECTION('ref_axis',(1.,0.,0.));
#7317=DIRECTION('center_axis',(0.,0.,1.));
#7318=DIRECTION('ref_axis',(1.,0.,0.));
#7319=DIRECTION('',(0.,0.,1.));
#7320=DIRECTION('center_axis',(0.,0.,1.));
#7321=DIRECTION('ref_axis',(1.,0.,0.));
#7322=DIRECTION('center_axis',(0.,0.,1.));
#7323=DIRECTION('ref_axis',(1.,0.,0.));
#7324=DIRECTION('',(0.,0.,-1.));
#7325=DIRECTION('center_axis',(0.,0.,1.));
#7326=DIRECTION('ref_axis',(1.,0.,0.));
#7327=DIRECTION('center_axis',(0.,0.,1.));
#7328=DIRECTION('ref_axis',(1.,0.,0.));
#7329=DIRECTION('center_axis',(0.,0.,-1.));
#7330=DIRECTION('ref_axis',(1.,0.,0.));
#7331=DIRECTION('center_axis',(0.,0.,1.));
#7332=DIRECTION('ref_axis',(1.,0.,0.));
#7333=DIRECTION('',(0.,0.,-1.));
#7334=DIRECTION('center_axis',(0.,0.,1.));
#7335=DIRECTION('ref_axis',(1.,0.,0.));
#7336=DIRECTION('',(0.,0.,-1.));
#7337=DIRECTION('center_axis',(0.,0.,1.));
#7338=DIRECTION('ref_axis',(1.,0.,0.));
#7339=DIRECTION('center_axis',(0.,0.,1.));
#7340=DIRECTION('ref_axis',(1.,0.,0.));
#7341=DIRECTION('axis',(0.,0.,1.));
#7342=DIRECTION('refdir',(1.,0.,0.));
#7343=DIRECTION('center_axis',(0.,1.,0.));
#7344=DIRECTION('ref_axis',(0.,0.,1.));
#7345=DIRECTION('center_axis',(0.,-1.,0.));
#7346=DIRECTION('ref_axis',(1.,0.,0.));
#7347=DIRECTION('center_axis',(0.,-1.,0.));
#7348=DIRECTION('ref_axis',(1.,0.,0.));
#7349=DIRECTION('center_axis',(0.,-1.,0.));
#7350=DIRECTION('ref_axis',(1.,0.,0.));
#7351=DIRECTION('',(0.707106781186548,0.707106781186547,8.65956056235493E-17));
#7352=DIRECTION('center_axis',(0.,-1.,0.));
#7353=DIRECTION('ref_axis',(1.,0.,0.));
#7354=DIRECTION('center_axis',(0.,-1.,0.));
#7355=DIRECTION('ref_axis',(1.,0.,0.));
#7356=DIRECTION('',(0.,1.,0.));
#7357=DIRECTION('center_axis',(0.,1.,0.));
#7358=DIRECTION('ref_axis',(1.,0.,0.));
#7359=DIRECTION('center_axis',(0.,-1.,0.));
#7360=DIRECTION('ref_axis',(1.,0.,0.));
#7361=DIRECTION('',(-0.707106781186547,0.707106781186548,-8.65956056235493E-17));
#7362=DIRECTION('center_axis',(0.,-1.,0.));
#7363=DIRECTION('ref_axis',(0.,0.,-1.));
#7364=DIRECTION('center_axis',(0.,-1.,0.));
#7365=DIRECTION('ref_axis',(1.,0.,0.));
#7366=DIRECTION('center_axis',(0.,1.,0.));
#7367=DIRECTION('ref_axis',(1.,0.,0.));
#7368=DIRECTION('center_axis',(0.,1.,0.));
#7369=DIRECTION('ref_axis',(1.,0.,0.));
#7370=DIRECTION('',(-0.447213595499958,0.894427190999916,-5.47678698264203E-17));
#7371=DIRECTION('center_axis',(0.,-1.,0.));
#7372=DIRECTION('ref_axis',(1.,0.,0.));
#7373=DIRECTION('center_axis',(0.,1.,0.));
#7374=DIRECTION('ref_axis',(1.,0.,0.));
#7375=DIRECTION('',(0.,1.,0.));
#7376=DIRECTION('center_axis',(0.,1.,0.));
#7377=DIRECTION('ref_axis',(1.,0.,0.));
#7378=DIRECTION('center_axis',(0.,-1.,0.));
#7379=DIRECTION('ref_axis',(1.,0.,0.));
#7380=DIRECTION('',(-0.707106781186547,0.707106781186548,-8.65956056235493E-17));
#7381=DIRECTION('center_axis',(0.,-1.,0.));
#7382=DIRECTION('ref_axis',(0.,0.,-1.));
#7383=DIRECTION('center_axis',(0.866025403784439,0.,-0.5));
#7384=DIRECTION('ref_axis',(0.5,0.,0.866025403784439));
#7385=DIRECTION('',(-0.5,0.,-0.866025403784439));
#7386=DIRECTION('',(0.,-1.,0.));
#7387=DIRECTION('',(0.5,0.,0.866025403784439));
#7388=DIRECTION('',(0.,-1.,0.));
#7389=DIRECTION('center_axis',(1.20185167898973E-16,0.,-1.));
#7390=DIRECTION('ref_axis',(1.,0.,1.20185167898973E-16));
#7391=DIRECTION('',(-1.,0.,-1.20185167898973E-16));
#7392=DIRECTION('',(0.,-1.,0.));
#7393=DIRECTION('',(1.,0.,1.20185167898973E-16));
#7394=DIRECTION('center_axis',(-0.866025403784439,0.,-0.5));
#7395=DIRECTION('ref_axis',(0.5,0.,-0.866025403784439));
#7396=DIRECTION('',(-0.5,0.,0.866025403784439));
#7397=DIRECTION('',(0.,-1.,0.));
#7398=DIRECTION('',(0.5,0.,-0.866025403784439));
#7399=DIRECTION('center_axis',(-0.866025403784439,0.,0.5));
#7400=DIRECTION('ref_axis',(-0.5,0.,-0.866025403784439));
#7401=DIRECTION('',(0.5,0.,0.866025403784439));
#7402=DIRECTION('',(0.,-1.,0.));
#7403=DIRECTION('',(-0.5,0.,-0.866025403784439));
#7404=DIRECTION('center_axis',(-2.40370335797945E-16,0.,1.));
#7405=DIRECTION('ref_axis',(-1.,0.,-2.40370335797945E-16));
#7406=DIRECTION('',(1.,0.,2.40370335797945E-16));
#7407=DIRECTION('',(0.,-1.,0.));
#7408=DIRECTION('',(-1.,0.,-2.40370335797945E-16));
#7409=DIRECTION('center_axis',(0.866025403784439,0.,0.5));
#7410=DIRECTION('ref_axis',(-0.5,0.,0.866025403784439));
#7411=DIRECTION('',(0.5,0.,-0.866025403784439));
#7412=DIRECTION('',(-0.5,0.,0.866025403784439));
#7413=DIRECTION('center_axis',(0.,1.,0.));
#7414=DIRECTION('ref_axis',(1.,0.,0.));
#7415=DIRECTION('center_axis',(0.,-1.,0.));
#7416=DIRECTION('ref_axis',(0.,0.,-1.));
#7417=DIRECTION('axis',(0.,0.,1.));
#7418=DIRECTION('refdir',(1.,0.,0.));
#7419=DIRECTION('axis',(0.,0.,1.));
#7420=DIRECTION('refdir',(1.,0.,0.));
#7421=DIRECTION('center_axis',(0.,-1.,0.));
#7422=DIRECTION('ref_axis',(0.,0.,-1.));
#7423=DIRECTION('center_axis',(0.,-1.,0.));
#7424=DIRECTION('ref_axis',(1.,0.,0.));
#7425=DIRECTION('center_axis',(0.,-1.,0.));
#7426=DIRECTION('ref_axis',(1.,0.,0.));
#7427=DIRECTION('center_axis',(1.,0.,1.22464679914735E-16));
#7428=DIRECTION('ref_axis',(-1.22464679914735E-16,0.,1.));
#7429=DIRECTION('center_axis',(0.,1.,0.));
#7430=DIRECTION('ref_axis',(1.,0.,0.));
#7431=DIRECTION('center_axis',(0.,1.,0.));
#7432=DIRECTION('ref_axis',(1.,0.,0.));
#7433=DIRECTION('center_axis',(0.,-1.,0.));
#7434=DIRECTION('ref_axis',(1.,0.,0.));
#7435=DIRECTION('',(0.,1.,0.));
#7436=DIRECTION('center_axis',(0.,-1.,0.));
#7437=DIRECTION('ref_axis',(1.,0.,0.));
#7438=DIRECTION('center_axis',(0.,-1.,0.));
#7439=DIRECTION('ref_axis',(1.,0.,0.));
#7440=DIRECTION('center_axis',(0.,-1.,0.));
#7441=DIRECTION('ref_axis',(1.,0.,0.));
#7442=DIRECTION('',(0.,1.,0.));
#7443=DIRECTION('center_axis',(0.,-1.,0.));
#7444=DIRECTION('ref_axis',(1.,0.,0.));
#7445=DIRECTION('center_axis',(0.,1.,0.));
#7446=DIRECTION('ref_axis',(1.,0.,0.));
#7447=DIRECTION('',(-0.707106781186547,0.707106781186548,-8.65956056235493E-17));
#7448=DIRECTION('center_axis',(0.,-1.,0.));
#7449=DIRECTION('ref_axis',(1.,0.,0.));
#7450=DIRECTION('center_axis',(0.,1.,0.));
#7451=DIRECTION('ref_axis',(0.,0.,1.));
#7452=DIRECTION('center_axis',(0.,-1.,0.));
#7453=DIRECTION('ref_axis',(1.,0.,0.));
#7454=DIRECTION('center_axis',(0.,-1.,0.));
#7455=DIRECTION('ref_axis',(1.,0.,0.));
#7456=DIRECTION('',(0.,1.,0.));
#7457=DIRECTION('center_axis',(0.,-1.,0.));
#7458=DIRECTION('ref_axis',(0.,0.,-1.));
#7459=DIRECTION('center_axis',(0.,-1.,0.));
#7460=DIRECTION('ref_axis',(1.,0.,0.));
#7461=DIRECTION('center_axis',(0.,-1.,0.));
#7462=DIRECTION('ref_axis',(1.,0.,0.));
#7463=DIRECTION('',(0.707106781186547,0.707106781186548,8.65956056235493E-17));
#7464=DIRECTION('axis',(0.,0.,1.));
#7465=DIRECTION('refdir',(1.,0.,0.));
#7466=DIRECTION('center_axis',(0.,-1.,0.));
#7467=DIRECTION('ref_axis',(0.,0.,-1.));
#7468=DIRECTION('center_axis',(0.,-1.,0.));
#7469=DIRECTION('ref_axis',(1.,0.,0.));
#7470=DIRECTION('center_axis',(0.,-1.,0.));
#7471=DIRECTION('ref_axis',(1.,0.,0.));
#7472=DIRECTION('center_axis',(1.,0.,1.22464679914735E-16));
#7473=DIRECTION('ref_axis',(-1.22464679914735E-16,0.,1.));
#7474=DIRECTION('center_axis',(0.,1.,0.));
#7475=DIRECTION('ref_axis',(1.,0.,0.));
#7476=DIRECTION('center_axis',(0.,1.,0.));
#7477=DIRECTION('ref_axis',(1.,0.,0.));
#7478=DIRECTION('center_axis',(0.,-1.,0.));
#7479=DIRECTION('ref_axis',(1.,0.,0.));
#7480=DIRECTION('center_axis',(0.,-1.,0.));
#7481=DIRECTION('ref_axis',(1.,0.,0.));
#7482=DIRECTION('',(0.,1.,0.));
#7483=DIRECTION('center_axis',(0.,1.,0.));
#7484=DIRECTION('ref_axis',(0.,0.,1.));
#7485=DIRECTION('center_axis',(0.,-1.,0.));
#7486=DIRECTION('ref_axis',(1.,0.,0.));
#7487=DIRECTION('center_axis',(0.,-1.,0.));
#7488=DIRECTION('ref_axis',(1.,0.,0.));
#7489=DIRECTION('center_axis',(0.,-1.,0.));
#7490=DIRECTION('ref_axis',(1.,0.,0.));
#7491=DIRECTION('center_axis',(0.,-1.,0.));
#7492=DIRECTION('ref_axis',(1.,0.,0.));
#7493=DIRECTION('',(0.707106781186548,0.707106781186547,8.65956056235494E-17));
#7494=DIRECTION('center_axis',(0.,-1.,0.));
#7495=DIRECTION('ref_axis',(1.,0.,0.));
#7496=DIRECTION('center_axis',(0.,-1.,0.));
#7497=DIRECTION('ref_axis',(1.,0.,0.));
#7498=DIRECTION('',(0.,1.,0.));
#7499=DIRECTION('center_axis',(0.,1.,0.));
#7500=DIRECTION('ref_axis',(1.,0.,0.));
#7501=DIRECTION('center_axis',(0.,-1.,0.));
#7502=DIRECTION('ref_axis',(1.,0.,0.));
#7503=DIRECTION('',(-0.707106781186548,0.707106781186547,-8.65956056235494E-17));
#7504=DIRECTION('center_axis',(0.,-1.,0.));
#7505=DIRECTION('ref_axis',(0.,0.,-1.));
#7506=DIRECTION('center_axis',(0.,-1.,0.));
#7507=DIRECTION('ref_axis',(1.,0.,0.));
#7508=DIRECTION('',(0.,1.,0.));
#7509=DIRECTION('axis',(0.,0.,1.));
#7510=DIRECTION('refdir',(1.,0.,0.));
#7511=DIRECTION('center_axis',(0.,0.,1.));
#7512=DIRECTION('ref_axis',(1.,0.,0.));
#7513=DIRECTION('center_axis',(1.22464679914735E-16,-1.,0.));
#7514=DIRECTION('ref_axis',(-1.,-1.22464679914735E-16,0.));
#7515=DIRECTION('center_axis',(0.707106781186548,0.,0.707106781186548));
#7516=DIRECTION('ref_axis',(0.707106781186548,0.,-0.707106781186548));
#7517=DIRECTION('center_axis',(8.65956056235494E-17,-1.,-8.65956056235493E-17));
#7518=DIRECTION('ref_axis',(-0.707106781186547,-1.22464679914735E-16,0.707106781186547));
#7519=DIRECTION('center_axis',(1.,0.,0.));
#7520=DIRECTION('ref_axis',(6.12323399573676E-17,0.,-1.));
#7521=DIRECTION('center_axis',(7.49879891330929E-33,-1.,-1.22464679914735E-16));
#7522=DIRECTION('ref_axis',(-6.12323399573676E-17,-1.22464679914735E-16,
1.));
#7523=DIRECTION('center_axis',(0.707106781186548,0.,-0.707106781186548));
#7524=DIRECTION('ref_axis',(-0.707106781186548,0.,-0.707106781186548));
#7525=DIRECTION('center_axis',(-8.65956056235493E-17,-1.,-8.65956056235494E-17));
#7526=DIRECTION('ref_axis',(0.707106781186547,-1.22464679914735E-16,0.707106781186547));
#7527=DIRECTION('center_axis',(0.,0.,-1.));
#7528=DIRECTION('ref_axis',(-1.,0.,-1.22464679914735E-16));
#7529=DIRECTION('center_axis',(-1.22464679914735E-16,-1.,-1.49975978266186E-32));
#7530=DIRECTION('ref_axis',(1.,-1.22464679914735E-16,1.22464679914735E-16));
#7531=DIRECTION('center_axis',(-0.707106781186547,0.,-0.707106781186548));
#7532=DIRECTION('ref_axis',(-0.707106781186548,0.,0.707106781186547));
#7533=DIRECTION('center_axis',(-8.65956056235493E-17,-1.,8.65956056235493E-17));
#7534=DIRECTION('ref_axis',(0.707106781186548,-1.22464679914735E-16,-0.707106781186547));
#7535=DIRECTION('center_axis',(-1.,0.,0.));
#7536=DIRECTION('ref_axis',(-1.83697019872103E-16,0.,1.));
#7537=DIRECTION('center_axis',(-2.24963967399279E-32,-1.,1.22464679914735E-16));
#7538=DIRECTION('ref_axis',(1.83697019872103E-16,-1.22464679914735E-16,
-1.));
#7539=DIRECTION('center_axis',(-0.707106781186548,0.,0.707106781186548));
#7540=DIRECTION('ref_axis',(0.707106781186547,0.,0.707106781186548));
#7541=DIRECTION('center_axis',(8.65956056235493E-17,-1.,8.65956056235493E-17));
#7542=DIRECTION('ref_axis',(-0.707106781186547,-1.22464679914735E-16,-0.707106781186548));
#7543=DIRECTION('axis',(0.,0.,1.));
#7544=DIRECTION('refdir',(1.,0.,0.));
#7545=DIRECTION('center_axis',(0.,0.,1.));
#7546=DIRECTION('ref_axis',(1.,0.,0.));
#7547=DIRECTION('center_axis',(0.,-1.,0.));
#7548=DIRECTION('ref_axis',(0.,0.,-1.));
#7549=DIRECTION('center_axis',(0.,-1.,0.));
#7550=DIRECTION('ref_axis',(0.,0.,-1.));
#7551=DIRECTION('center_axis',(0.,1.,0.));
#7552=DIRECTION('ref_axis',(1.,0.,0.));
#7553=DIRECTION('center_axis',(0.,1.,0.));
#7554=DIRECTION('ref_axis',(1.,0.,0.));
#7555=DIRECTION('center_axis',(0.,1.,0.));
#7556=DIRECTION('ref_axis',(1.,0.,0.));
#7557=DIRECTION('center_axis',(0.,1.,0.));
#7558=DIRECTION('ref_axis',(1.,0.,0.));
#7559=DIRECTION('',(0.,-1.,0.));
#7560=DIRECTION('center_axis',(0.,-1.,0.));
#7561=DIRECTION('ref_axis',(1.,0.,0.));
#7562=DIRECTION('center_axis',(0.,1.,0.));
#7563=DIRECTION('ref_axis',(1.,0.,0.));
#7564=DIRECTION('center_axis',(0.,1.,0.));
#7565=DIRECTION('ref_axis',(1.,0.,0.));
#7566=DIRECTION('center_axis',(0.,1.,0.));
#7567=DIRECTION('ref_axis',(1.,0.,0.));
#7568=DIRECTION('center_axis',(0.,1.,0.));
#7569=DIRECTION('ref_axis',(1.,0.,0.));
#7570=DIRECTION('center_axis',(0.,1.,0.));
#7571=DIRECTION('ref_axis',(1.,0.,0.));
#7572=DIRECTION('center_axis',(0.,1.,0.));
#7573=DIRECTION('ref_axis',(1.,0.,0.));
#7574=DIRECTION('center_axis',(0.,-1.,0.));
#7575=DIRECTION('ref_axis',(1.,0.,0.));
#7576=DIRECTION('center_axis',(0.,-1.,0.));
#7577=DIRECTION('ref_axis',(0.,0.,-1.));
#7578=DIRECTION('center_axis',(6.12323399573677E-17,0.,1.));
#7579=DIRECTION('ref_axis',(1.,0.,0.));
#7580=DIRECTION('center_axis',(0.,-1.,0.));
#7581=DIRECTION('ref_axis',(0.,0.,-1.));
#7582=DIRECTION('center_axis',(0.,1.,0.));
#7583=DIRECTION('ref_axis',(1.,0.,0.));
#7584=DIRECTION('center_axis',(0.,-1.,0.));
#7585=DIRECTION('ref_axis',(1.,0.,0.));
#7586=DIRECTION('center_axis',(0.,-1.,0.));
#7587=DIRECTION('ref_axis',(0.,0.,-1.));
#7588=DIRECTION('center_axis',(0.,0.,1.));
#7589=DIRECTION('ref_axis',(1.,0.,0.));
#7590=DIRECTION('center_axis',(0.,-1.,0.));
#7591=DIRECTION('ref_axis',(0.,0.,-1.));
#7592=DIRECTION('center_axis',(0.,1.,0.));
#7593=DIRECTION('ref_axis',(1.,0.,0.));
#7594=DIRECTION('center_axis',(0.,-1.,0.));
#7595=DIRECTION('ref_axis',(1.,0.,0.));
#7596=DIRECTION('center_axis',(0.,-1.,0.));
#7597=DIRECTION('ref_axis',(0.,0.,-1.));
#7598=DIRECTION('center_axis',(0.,0.,1.));
#7599=DIRECTION('ref_axis',(1.,0.,0.));
#7600=DIRECTION('center_axis',(0.,-1.,0.));
#7601=DIRECTION('ref_axis',(0.,0.,-1.));
#7602=DIRECTION('center_axis',(0.,1.,0.));
#7603=DIRECTION('ref_axis',(1.,0.,0.));
#7604=DIRECTION('center_axis',(0.,-1.,0.));
#7605=DIRECTION('ref_axis',(1.,0.,0.));
#7606=DIRECTION('center_axis',(0.,-1.,0.));
#7607=DIRECTION('ref_axis',(0.,0.,-1.));
#7608=DIRECTION('center_axis',(0.,0.,1.));
#7609=DIRECTION('ref_axis',(1.,0.,0.));
#7610=DIRECTION('center_axis',(0.,-1.,0.));
#7611=DIRECTION('ref_axis',(0.,0.,-1.));
#7612=DIRECTION('center_axis',(0.,1.,0.));
#7613=DIRECTION('ref_axis',(1.,0.,0.));
#7614=DIRECTION('center_axis',(0.,-1.,0.));
#7615=DIRECTION('ref_axis',(1.,0.,0.));
#7616=DIRECTION('center_axis',(0.,-1.,0.));
#7617=DIRECTION('ref_axis',(0.,0.,-1.));
#7618=DIRECTION('center_axis',(6.12323399573676E-17,0.,1.));
#7619=DIRECTION('ref_axis',(1.,0.,0.));
#7620=DIRECTION('center_axis',(0.,-1.,0.));
#7621=DIRECTION('ref_axis',(0.,0.,-1.));
#7622=DIRECTION('center_axis',(0.,1.,0.));
#7623=DIRECTION('ref_axis',(1.,0.,0.));
#7624=DIRECTION('center_axis',(0.,-1.,0.));
#7625=DIRECTION('ref_axis',(1.,0.,0.));
#7626=DIRECTION('center_axis',(0.,-1.,0.));
#7627=DIRECTION('ref_axis',(0.,0.,-1.));
#7628=DIRECTION('center_axis',(0.,0.,1.));
#7629=DIRECTION('ref_axis',(1.,0.,0.));
#7630=DIRECTION('center_axis',(0.,-1.,0.));
#7631=DIRECTION('ref_axis',(0.,0.,-1.));
#7632=DIRECTION('center_axis',(0.,1.,0.));
#7633=DIRECTION('ref_axis',(1.,0.,0.));
#7634=DIRECTION('center_axis',(0.,1.,0.));
#7635=DIRECTION('ref_axis',(1.,0.,0.));
#7636=DIRECTION('',(0.,1.,0.));
#7637=DIRECTION('center_axis',(0.,-1.,0.));
#7638=DIRECTION('ref_axis',(1.,0.,0.));
#7639=DIRECTION('center_axis',(0.,-1.,0.));
#7640=DIRECTION('ref_axis',(1.,0.,0.));
#7641=DIRECTION('center_axis',(0.,1.,0.));
#7642=DIRECTION('ref_axis',(1.,0.,0.));
#7643=DIRECTION('center_axis',(0.,-1.,0.));
#7644=DIRECTION('ref_axis',(0.,0.,-1.));
#7645=DIRECTION('center_axis',(0.,0.,1.));
#7646=DIRECTION('ref_axis',(1.,0.,0.));
#7647=DIRECTION('center_axis',(0.,-1.,0.));
#7648=DIRECTION('ref_axis',(0.,0.,-1.));
#7649=DIRECTION('center_axis',(0.,-1.,0.));
#7650=DIRECTION('ref_axis',(-1.,0.,0.));
#7651=DIRECTION('center_axis',(0.,1.,0.));
#7652=DIRECTION('ref_axis',(1.,0.,0.));
#7653=DIRECTION('axis',(0.,0.,1.));
#7654=DIRECTION('refdir',(1.,0.,0.));
#7655=DIRECTION('center_axis',(0.,1.,0.));
#7656=DIRECTION('ref_axis',(0.,0.,1.));
#7657=DIRECTION('center_axis',(0.,-1.,0.));
#7658=DIRECTION('ref_axis',(1.,0.,0.));
#7659=DIRECTION('center_axis',(0.,-1.,0.));
#7660=DIRECTION('ref_axis',(1.,0.,0.));
#7661=DIRECTION('center_axis',(0.,-1.,0.));
#7662=DIRECTION('ref_axis',(1.,0.,0.));
#7663=DIRECTION('center_axis',(0.,-1.,0.));
#7664=DIRECTION('ref_axis',(1.,0.,0.));
#7665=DIRECTION('',(0.,1.,0.));
#7666=DIRECTION('center_axis',(0.,-1.,0.));
#7667=DIRECTION('ref_axis',(0.,0.,-1.));
#7668=DIRECTION('center_axis',(0.,-1.,0.));
#7669=DIRECTION('ref_axis',(1.,0.,0.));
#7670=DIRECTION('center_axis',(0.,-1.,0.));
#7671=DIRECTION('ref_axis',(1.,0.,0.));
#7672=DIRECTION('',(0.,1.,0.));
#7673=DIRECTION('center_axis',(0.,1.,0.));
#7674=DIRECTION('ref_axis',(0.,0.,1.));
#7675=DIRECTION('center_axis',(0.,-1.,0.));
#7676=DIRECTION('ref_axis',(1.,0.,0.));
#7677=DIRECTION('center_axis',(0.,-1.,0.));
#7678=DIRECTION('ref_axis',(1.,0.,0.));
#7679=DIRECTION('center_axis',(0.,-1.,0.));
#7680=DIRECTION('ref_axis',(1.,0.,0.));
#7681=DIRECTION('center_axis',(0.,-1.,0.));
#7682=DIRECTION('ref_axis',(1.,0.,0.));
#7683=DIRECTION('',(0.,1.,0.));
#7684=DIRECTION('center_axis',(0.,-1.,0.));
#7685=DIRECTION('ref_axis',(0.,0.,-1.));
#7686=DIRECTION('center_axis',(0.,-1.,0.));
#7687=DIRECTION('ref_axis',(1.,0.,0.));
#7688=DIRECTION('center_axis',(0.,-1.,0.));
#7689=DIRECTION('ref_axis',(1.,0.,0.));
#7690=DIRECTION('',(0.,1.,0.));
#7691=DIRECTION('',(0.,0.,1.));
#7692=DIRECTION('',(1.,0.,0.));
#7693=DIRECTION('',(0.,0.,1.));
#7694=DIRECTION('',(1.,0.,0.));
#7695=DIRECTION('',(0.,0.,1.));
#7696=DIRECTION('',(1.,0.,0.));
#7697=DIRECTION('',(0.,0.,1.));
#7698=DIRECTION('',(1.,0.,0.));
#7699=DIRECTION('',(0.,0.,1.));
#7700=DIRECTION('',(1.,0.,0.));
#7701=DIRECTION('axis',(0.,0.,1.));
#7702=DIRECTION('refdir',(1.,0.,0.));
#7703=DIRECTION('axis',(0.,0.,1.));
#7704=DIRECTION('refdir',(1.,0.,0.));
#7705=DIRECTION('center_axis',(0.,0.,1.));
#7706=DIRECTION('ref_axis',(1.,0.,0.));
#7707=DIRECTION('center_axis',(0.,0.,1.));
#7708=DIRECTION('ref_axis',(1.,0.,0.));
#7709=DIRECTION('',(0.,0.,1.));
#7710=DIRECTION('center_axis',(0.,0.,-1.));
#7711=DIRECTION('ref_axis',(1.,0.,0.));
#7712=DIRECTION('center_axis',(0.,0.,1.));
#7713=DIRECTION('ref_axis',(1.,0.,0.));
#7714=DIRECTION('center_axis',(0.,0.,1.));
#7715=DIRECTION('ref_axis',(1.,0.,0.));
#7716=DIRECTION('center_axis',(0.,0.,1.));
#7717=DIRECTION('ref_axis',(1.,0.,0.));
#7718=DIRECTION('',(0.,0.,1.));
#7719=DIRECTION('center_axis',(0.,0.,-1.));
#7720=DIRECTION('ref_axis',(1.,0.,0.));
#7721=DIRECTION('center_axis',(0.,0.,1.));
#7722=DIRECTION('ref_axis',(1.,0.,0.));
#7723=DIRECTION('',(0.,0.,1.));
#7724=DIRECTION('center_axis',(0.,0.,1.));
#7725=DIRECTION('ref_axis',(1.,0.,0.));
#7726=DIRECTION('',(0.,0.,1.));
#7727=DIRECTION('center_axis',(0.,0.,1.));
#7728=DIRECTION('ref_axis',(1.,0.,0.));
#7729=DIRECTION('center_axis',(0.,0.,1.));
#7730=DIRECTION('ref_axis',(1.,0.,0.));
#7731=DIRECTION('',(1.,0.,0.));
#7732=DIRECTION('center_axis',(0.,0.,1.));
#7733=DIRECTION('ref_axis',(1.,0.,0.));
#7734=DIRECTION('',(1.,0.,0.));
#7735=DIRECTION('',(0.,-1.,0.));
#7736=DIRECTION('',(-1.,0.,0.));
#7737=DIRECTION('center_axis',(0.,0.,1.));
#7738=DIRECTION('ref_axis',(1.,0.,0.));
#7739=DIRECTION('',(-1.,0.,0.));
#7740=DIRECTION('center_axis',(0.,0.,1.));
#7741=DIRECTION('ref_axis',(1.,0.,0.));
#7742=DIRECTION('center_axis',(0.,1.,0.));
#7743=DIRECTION('ref_axis',(-1.,0.,0.));
#7744=DIRECTION('',(0.,0.,-1.));
#7745=DIRECTION('',(-1.,0.,0.));
#7746=DIRECTION('center_axis',(0.,-1.,0.));
#7747=DIRECTION('ref_axis',(1.,0.,0.));
#7748=DIRECTION('',(0.,0.,1.));
#7749=DIRECTION('',(1.,0.,0.));
#7750=DIRECTION('center_axis',(0.,-1.,0.));
#7751=DIRECTION('ref_axis',(1.,0.,0.));
#7752=DIRECTION('',(0.,0.,-1.));
#7753=DIRECTION('',(1.,0.,0.));
#7754=DIRECTION('',(0.,0.,1.));
#7755=DIRECTION('center_axis',(0.,1.,0.));
#7756=DIRECTION('ref_axis',(-1.,0.,0.));
#7757=DIRECTION('',(0.,0.,1.));
#7758=DIRECTION('',(0.,0.,1.));
#7759=DIRECTION('',(-1.,0.,0.));
#7760=DIRECTION('center_axis',(-1.,0.,0.));
#7761=DIRECTION('ref_axis',(0.,-1.,0.));
#7762=DIRECTION('',(0.,-1.,0.));
#7763=DIRECTION('center_axis',(0.,0.,1.));
#7764=DIRECTION('ref_axis',(1.,0.,0.));
#7765=DIRECTION('center_axis',(0.,0.,1.));
#7766=DIRECTION('ref_axis',(1.,0.,0.));
#7767=DIRECTION('center_axis',(0.,0.,1.));
#7768=DIRECTION('ref_axis',(1.,0.,0.));
#7769=DIRECTION('center_axis',(0.,0.,1.));
#7770=DIRECTION('ref_axis',(1.,0.,0.));
#7771=DIRECTION('center_axis',(0.,0.,1.));
#7772=DIRECTION('ref_axis',(1.,0.,0.));
#7773=DIRECTION('center_axis',(0.,0.,1.));
#7774=DIRECTION('ref_axis',(1.,0.,0.));
#7775=DIRECTION('center_axis',(0.,0.,1.));
#7776=DIRECTION('ref_axis',(1.,0.,0.));
#7777=DIRECTION('center_axis',(0.,0.,1.));
#7778=DIRECTION('ref_axis',(1.,0.,0.));
#7779=DIRECTION('center_axis',(0.,0.,-1.));
#7780=DIRECTION('ref_axis',(1.,0.,0.));
#7781=DIRECTION('center_axis',(0.,0.,1.));
#7782=DIRECTION('ref_axis',(1.,0.,0.));
#7783=DIRECTION('',(0.,0.,-1.));
#7784=DIRECTION('center_axis',(0.,0.,1.));
#7785=DIRECTION('ref_axis',(1.,0.,0.));
#7786=DIRECTION('',(0.,0.,-1.));
#7787=DIRECTION('center_axis',(0.,0.,1.));
#7788=DIRECTION('ref_axis',(1.,0.,0.));
#7789=DIRECTION('center_axis',(0.,0.,1.));
#7790=DIRECTION('ref_axis',(1.,0.,0.));
#7791=DIRECTION('center_axis',(0.,0.,1.));
#7792=DIRECTION('ref_axis',(1.,0.,0.));
#7793=DIRECTION('',(0.,0.,-1.));
#7794=DIRECTION('center_axis',(0.,0.,1.));
#7795=DIRECTION('ref_axis',(1.,0.,0.));
#7796=DIRECTION('center_axis',(0.,0.,1.));
#7797=DIRECTION('ref_axis',(1.,0.,0.));
#7798=DIRECTION('axis',(0.,0.,1.));
#7799=DIRECTION('refdir',(1.,0.,0.));
#7800=DIRECTION('center_axis',(0.,0.,1.));
#7801=DIRECTION('ref_axis',(1.,0.,0.));
#7802=DIRECTION('center_axis',(0.,0.,-1.));
#7803=DIRECTION('ref_axis',(1.,0.,0.));
#7804=DIRECTION('',(0.,0.,-1.));
#7805=DIRECTION('center_axis',(0.,0.,-1.));
#7806=DIRECTION('ref_axis',(1.,0.,0.));
#7807=DIRECTION('center_axis',(0.,0.,1.));
#7808=DIRECTION('ref_axis',(1.,0.,0.));
#7809=DIRECTION('center_axis',(0.,0.,1.));
#7810=DIRECTION('ref_axis',(1.,0.,0.));
#7811=DIRECTION('',(0.,0.,-1.));
#7812=DIRECTION('center_axis',(0.,0.,1.));
#7813=DIRECTION('ref_axis',(1.,0.,0.));
#7814=DIRECTION('center_axis',(0.,0.,1.));
#7815=DIRECTION('ref_axis',(1.,0.,0.));
#7816=DIRECTION('center_axis',(0.,0.,1.));
#7817=DIRECTION('ref_axis',(1.,0.,0.));
#7818=DIRECTION('axis',(0.,0.,1.));
#7819=DIRECTION('refdir',(1.,0.,0.));
#7820=DIRECTION('center_axis',(0.,1.,0.));
#7821=DIRECTION('ref_axis',(1.,0.,0.));
#7822=DIRECTION('',(0.,0.,-1.));
#7823=DIRECTION('center_axis',(0.,1.,0.));
#7824=DIRECTION('ref_axis',(1.,0.,0.));
#7825=DIRECTION('center_axis',(0.,1.,0.));
#7826=DIRECTION('ref_axis',(1.,0.,0.));
#7827=DIRECTION('center_axis',(0.,1.,0.));
#7828=DIRECTION('ref_axis',(1.,0.,0.));
#7829=DIRECTION('',(0.,1.,0.));
#7830=DIRECTION('center_axis',(0.,1.,0.));
#7831=DIRECTION('ref_axis',(1.,0.,0.));
#7832=DIRECTION('center_axis',(0.,1.,0.));
#7833=DIRECTION('ref_axis',(1.,0.,0.));
#7834=DIRECTION('',(0.,0.,1.));
#7835=DIRECTION('center_axis',(1.,0.,0.));
#7836=DIRECTION('ref_axis',(0.,0.,-1.));
#7837=DIRECTION('',(0.,0.,-1.));
#7838=DIRECTION('center_axis',(1.,0.,0.));
#7839=DIRECTION('ref_axis',(0.,0.,-1.));
#7840=DIRECTION('center_axis',(1.,0.,0.));
#7841=DIRECTION('ref_axis',(0.,0.,-1.));
#7842=DIRECTION('',(1.,0.,0.));
#7843=DIRECTION('center_axis',(1.,0.,0.));
#7844=DIRECTION('ref_axis',(0.,0.,-1.));
#7845=DIRECTION('center_axis',(1.,0.,0.));
#7846=DIRECTION('ref_axis',(0.,0.,-1.));
#7847=DIRECTION('',(0.,0.,1.));
#7848=DIRECTION('center_axis',(0.,0.,1.));
#7849=DIRECTION('ref_axis',(1.,0.,0.));
#7850=DIRECTION('center_axis',(0.,0.,-1.));
#7851=DIRECTION('ref_axis',(1.,0.,0.));
#7852=DIRECTION('',(0.,0.,-1.));
#7853=DIRECTION('',(0.,0.,-1.));
#7854=DIRECTION('center_axis',(0.,0.,-1.));
#7855=DIRECTION('ref_axis',(1.,0.,0.));
#7856=DIRECTION('center_axis',(0.,0.,1.));
#7857=DIRECTION('ref_axis',(1.,0.,0.));
#7858=DIRECTION('center_axis',(0.,0.,1.));
#7859=DIRECTION('ref_axis',(1.,0.,0.));
#7860=DIRECTION('',(0.,0.,-1.));
#7861=DIRECTION('',(0.,0.,-1.));
#7862=DIRECTION('center_axis',(0.,0.,1.));
#7863=DIRECTION('ref_axis',(1.,0.,0.));
#7864=DIRECTION('center_axis',(0.,0.,1.));
#7865=DIRECTION('ref_axis',(1.,0.,0.));
#7866=DIRECTION('center_axis',(0.,0.,1.));
#7867=DIRECTION('ref_axis',(1.,0.,0.));
#7868=DIRECTION('axis',(0.,0.,1.));
#7869=DIRECTION('refdir',(1.,0.,0.));
#7870=DIRECTION('center_axis',(0.,0.,1.));
#7871=DIRECTION('ref_axis',(1.,0.,0.));
#7872=DIRECTION('center_axis',(0.,0.,1.));
#7873=DIRECTION('ref_axis',(1.,0.,0.));
#7874=DIRECTION('center_axis',(0.,0.,1.));
#7875=DIRECTION('ref_axis',(1.,0.,0.));
#7876=DIRECTION('center_axis',(0.,0.,1.));
#7877=DIRECTION('ref_axis',(1.,0.,0.));
#7878=DIRECTION('center_axis',(0.,0.,1.));
#7879=DIRECTION('ref_axis',(1.,0.,0.));
#7880=DIRECTION('center_axis',(0.,0.,-1.));
#7881=DIRECTION('ref_axis',(1.,0.,0.));
#7882=DIRECTION('center_axis',(0.,0.,1.));
#7883=DIRECTION('ref_axis',(1.,0.,0.));
#7884=DIRECTION('',(0.,0.,-1.));
#7885=DIRECTION('center_axis',(0.,0.,1.));
#7886=DIRECTION('ref_axis',(1.,0.,0.));
#7887=DIRECTION('',(0.,0.,-1.));
#7888=DIRECTION('center_axis',(0.,0.,1.));
#7889=DIRECTION('ref_axis',(1.,0.,0.));
#7890=DIRECTION('center_axis',(0.,0.,1.));
#7891=DIRECTION('ref_axis',(1.,0.,0.));
#7892=DIRECTION('center_axis',(0.,0.,1.));
#7893=DIRECTION('ref_axis',(1.,0.,0.));
#7894=DIRECTION('',(0.,0.,-1.));
#7895=DIRECTION('center_axis',(0.,0.,1.));
#7896=DIRECTION('ref_axis',(1.,0.,0.));
#7897=DIRECTION('center_axis',(0.,0.,1.));
#7898=DIRECTION('ref_axis',(1.,0.,0.));
#7899=DIRECTION('axis',(0.,0.,1.));
#7900=DIRECTION('refdir',(1.,0.,0.));
#7901=DIRECTION('center_axis',(0.,0.,1.));
#7902=DIRECTION('ref_axis',(1.,0.,0.));
#7903=DIRECTION('center_axis',(0.,0.,1.));
#7904=DIRECTION('ref_axis',(1.,0.,0.));
#7905=DIRECTION('',(0.,0.,1.));
#7906=DIRECTION('center_axis',(0.,0.,-1.));
#7907=DIRECTION('ref_axis',(1.,0.,0.));
#7908=DIRECTION('center_axis',(0.,0.,1.));
#7909=DIRECTION('ref_axis',(1.,0.,0.));
#7910=DIRECTION('',(0.,0.,-1.));
#7911=DIRECTION('center_axis',(0.,0.,1.));
#7912=DIRECTION('ref_axis',(1.,0.,0.));
#7913=DIRECTION('',(0.,0.,1.));
#7914=DIRECTION('center_axis',(0.,0.,1.));
#7915=DIRECTION('ref_axis',(1.,0.,0.));
#7916=DIRECTION('center_axis',(0.,0.,1.));
#7917=DIRECTION('ref_axis',(1.,0.,0.));
#7918=DIRECTION('',(0.,-1.,0.));
#7919=DIRECTION('center_axis',(0.,0.,1.));
#7920=DIRECTION('ref_axis',(1.,0.,0.));
#7921=DIRECTION('',(0.,-1.,0.));
#7922=DIRECTION('center_axis',(-1.,0.,0.));
#7923=DIRECTION('ref_axis',(0.,-1.,0.));
#7924=DIRECTION('',(0.,1.,0.));
#7925=DIRECTION('',(0.,0.,1.));
#7926=DIRECTION('center_axis',(-1.,0.,0.));
#7927=DIRECTION('ref_axis',(0.,-1.,0.));
#7928=DIRECTION('',(0.,0.,-1.));
#7929=DIRECTION('',(0.,1.,0.));
#7930=DIRECTION('center_axis',(0.,0.,1.));
#7931=DIRECTION('ref_axis',(-1.,1.22464679914735E-16,0.));
#7932=DIRECTION('center_axis',(0.,0.,1.));
#7933=DIRECTION('ref_axis',(1.,0.,0.));
#7934=DIRECTION('center_axis',(0.,0.,1.));
#7935=DIRECTION('ref_axis',(1.,0.,0.));
#7936=DIRECTION('axis',(0.,0.,1.));
#7937=DIRECTION('refdir',(1.,0.,0.));
#7938=DIRECTION('center_axis',(0.,0.,1.));
#7939=DIRECTION('ref_axis',(1.,0.,0.));
#7940=DIRECTION('center_axis',(0.,0.,-1.));
#7941=DIRECTION('ref_axis',(1.,0.,0.));
#7942=DIRECTION('',(0.,0.,-1.));
#7943=DIRECTION('center_axis',(0.,0.,-1.));
#7944=DIRECTION('ref_axis',(1.,0.,0.));
#7945=DIRECTION('center_axis',(0.,0.,1.));
#7946=DIRECTION('ref_axis',(1.,0.,0.));
#7947=DIRECTION('center_axis',(0.,0.,1.));
#7948=DIRECTION('ref_axis',(1.,0.,0.));
#7949=DIRECTION('',(0.,0.,-1.));
#7950=DIRECTION('center_axis',(0.,0.,1.));
#7951=DIRECTION('ref_axis',(1.,0.,0.));
#7952=DIRECTION('center_axis',(0.,0.,1.));
#7953=DIRECTION('ref_axis',(1.,0.,0.));
#7954=DIRECTION('center_axis',(0.,0.,1.));
#7955=DIRECTION('ref_axis',(1.,0.,0.));
#7956=DIRECTION('axis',(0.,0.,1.));
#7957=DIRECTION('refdir',(1.,0.,0.));
#7958=DIRECTION('center_axis',(0.,0.,1.));
#7959=DIRECTION('ref_axis',(1.,0.,0.));
#7960=DIRECTION('center_axis',(0.,0.,-1.));
#7961=DIRECTION('ref_axis',(1.,0.,0.));
#7962=DIRECTION('',(0.,0.,-1.));
#7963=DIRECTION('center_axis',(0.,0.,-1.));
#7964=DIRECTION('ref_axis',(1.,0.,0.));
#7965=DIRECTION('center_axis',(0.,0.,1.));
#7966=DIRECTION('ref_axis',(1.,0.,0.));
#7967=DIRECTION('center_axis',(0.,0.,1.));
#7968=DIRECTION('ref_axis',(1.,0.,0.));
#7969=DIRECTION('',(0.,0.,-1.));
#7970=DIRECTION('center_axis',(0.,0.,1.));
#7971=DIRECTION('ref_axis',(1.,0.,0.));
#7972=DIRECTION('center_axis',(0.,0.,1.));
#7973=DIRECTION('ref_axis',(1.,0.,0.));
#7974=DIRECTION('center_axis',(0.,0.,1.));
#7975=DIRECTION('ref_axis',(1.,0.,0.));
#7976=DIRECTION('axis',(0.,0.,1.));
#7977=DIRECTION('refdir',(1.,0.,0.));
#7978=DIRECTION('center_axis',(0.,0.,1.));
#7979=DIRECTION('ref_axis',(1.,0.,0.));
#7980=DIRECTION('center_axis',(0.,0.,-1.));
#7981=DIRECTION('ref_axis',(1.,0.,0.));
#7982=DIRECTION('',(0.,0.,-1.));
#7983=DIRECTION('center_axis',(0.,0.,-1.));
#7984=DIRECTION('ref_axis',(1.,0.,0.));
#7985=DIRECTION('center_axis',(0.,0.,1.));
#7986=DIRECTION('ref_axis',(1.,0.,0.));
#7987=DIRECTION('center_axis',(0.,0.,1.));
#7988=DIRECTION('ref_axis',(1.,0.,0.));
#7989=DIRECTION('',(0.,0.,-1.));
#7990=DIRECTION('center_axis',(0.,0.,1.));
#7991=DIRECTION('ref_axis',(1.,0.,0.));
#7992=DIRECTION('center_axis',(0.,0.,1.));
#7993=DIRECTION('ref_axis',(1.,0.,0.));
#7994=DIRECTION('center_axis',(0.,0.,1.));
#7995=DIRECTION('ref_axis',(1.,0.,0.));
#7996=DIRECTION('axis',(0.,0.,1.));
#7997=DIRECTION('refdir',(1.,0.,0.));
#7998=DIRECTION('center_axis',(0.866025403784439,0.,-0.5));
#7999=DIRECTION('ref_axis',(0.5,0.,0.866025403784439));
#8000=DIRECTION('',(-0.5,0.,-0.866025403784439));
#8001=DIRECTION('',(0.,-1.,0.));
#8002=DIRECTION('',(0.5,0.,0.866025403784439));
#8003=DIRECTION('',(0.,-1.,0.));
#8004=DIRECTION('center_axis',(1.60246890531964E-16,0.,-1.));
#8005=DIRECTION('ref_axis',(1.,0.,1.60246890531964E-16));
#8006=DIRECTION('',(-1.,0.,-1.60246890531964E-16));
#8007=DIRECTION('',(0.,-1.,0.));
#8008=DIRECTION('',(1.,0.,1.60246890531964E-16));
#8009=DIRECTION('center_axis',(-0.866025403784439,0.,-0.5));
#8010=DIRECTION('ref_axis',(0.5,0.,-0.866025403784439));
#8011=DIRECTION('',(-0.5,0.,0.866025403784439));
#8012=DIRECTION('',(0.,-1.,0.));
#8013=DIRECTION('',(0.5,0.,-0.866025403784439));
#8014=DIRECTION('center_axis',(-0.866025403784439,0.,0.5));
#8015=DIRECTION('ref_axis',(-0.5,0.,-0.866025403784439));
#8016=DIRECTION('',(0.5,0.,0.866025403784439));
#8017=DIRECTION('',(0.,-1.,0.));
#8018=DIRECTION('',(-0.5,0.,-0.866025403784439));
#8019=DIRECTION('center_axis',(-1.60246890531964E-16,0.,1.));
#8020=DIRECTION('ref_axis',(-1.,0.,-1.60246890531964E-16));
#8021=DIRECTION('',(1.,0.,1.60246890531964E-16));
#8022=DIRECTION('',(0.,-1.,0.));
#8023=DIRECTION('',(-1.,0.,-1.60246890531964E-16));
#8024=DIRECTION('center_axis',(0.866025403784439,0.,0.5));
#8025=DIRECTION('ref_axis',(-0.5,0.,0.866025403784439));
#8026=DIRECTION('',(0.5,0.,-0.866025403784439));
#8027=DIRECTION('',(-0.5,0.,0.866025403784439));
#8028=DIRECTION('center_axis',(0.,1.,0.));
#8029=DIRECTION('ref_axis',(1.,0.,0.));
#8030=DIRECTION('center_axis',(0.,-1.,0.));
#8031=DIRECTION('ref_axis',(0.,0.,-1.));
#8032=DIRECTION('center_axis',(0.,1.,0.));
#8033=DIRECTION('ref_axis',(1.,0.,0.));
#8034=DIRECTION('center_axis',(0.,1.,0.));
#8035=DIRECTION('ref_axis',(1.,0.,0.));
#8036=DIRECTION('center_axis',(0.,1.,0.));
#8037=DIRECTION('ref_axis',(0.,0.,1.));
#8038=DIRECTION('center_axis',(0.,-1.,0.));
#8039=DIRECTION('ref_axis',(1.,0.,0.));
#8040=DIRECTION('center_axis',(0.,-1.,0.));
#8041=DIRECTION('ref_axis',(1.,0.,0.));
#8042=DIRECTION('center_axis',(0.,-1.,0.));
#8043=DIRECTION('ref_axis',(1.,0.,0.));
#8044=DIRECTION('',(0.707106781186547,0.707106781186548,8.65956056235493E-17));
#8045=DIRECTION('center_axis',(0.,-1.,0.));
#8046=DIRECTION('ref_axis',(1.,0.,0.));
#8047=DIRECTION('center_axis',(0.,-1.,0.));
#8048=DIRECTION('ref_axis',(1.,0.,0.));
#8049=DIRECTION('',(0.,1.,0.));
#8050=DIRECTION('center_axis',(0.,1.,0.));
#8051=DIRECTION('ref_axis',(1.,0.,0.));
#8052=DIRECTION('center_axis',(0.,-1.,0.));
#8053=DIRECTION('ref_axis',(1.,0.,0.));
#8054=DIRECTION('',(-0.707106781186547,0.707106781186548,-8.65956056235493E-17));
#8055=DIRECTION('center_axis',(0.,-1.,0.));
#8056=DIRECTION('ref_axis',(0.,0.,-1.));
#8057=DIRECTION('center_axis',(0.,-1.,0.));
#8058=DIRECTION('ref_axis',(1.,0.,0.));
#8059=DIRECTION('center_axis',(0.,1.,0.));
#8060=DIRECTION('ref_axis',(1.,0.,0.));
#8061=DIRECTION('center_axis',(0.,1.,0.));
#8062=DIRECTION('ref_axis',(1.,0.,0.));
#8063=DIRECTION('',(-0.447213595499958,0.894427190999916,-5.47678698264203E-17));
#8064=DIRECTION('center_axis',(0.,-1.,0.));
#8065=DIRECTION('ref_axis',(1.,0.,0.));
#8066=DIRECTION('',(0.,1.,0.));
#8067=DIRECTION('',(0.,0.,1.));
#8068=DIRECTION('',(1.,0.,0.));
#8069=DIRECTION('',(0.,0.,1.));
#8070=DIRECTION('',(1.,0.,0.));
#8071=DIRECTION('',(0.,0.,1.));
#8072=DIRECTION('',(1.,0.,0.));
#8073=DIRECTION('',(0.,0.,1.));
#8074=DIRECTION('',(1.,0.,0.));
#8075=DIRECTION('',(0.,0.,1.));
#8076=DIRECTION('',(1.,0.,0.));
#8077=DIRECTION('',(0.,0.,1.));
#8078=DIRECTION('',(1.,0.,0.));
#8079=DIRECTION('',(0.,-1.,2.22044604925031E-16));
#8080=DIRECTION('',(1.,0.,0.));
#8081=DIRECTION('',(0.,-1.,2.22044604925031E-16));
#8082=DIRECTION('',(1.,0.,0.));
#8083=DIRECTION('',(0.,-1.,2.22044604925031E-16));
#8084=DIRECTION('',(1.,0.,0.));
#8085=DIRECTION('',(0.,-1.,2.22044604925031E-16));
#8086=DIRECTION('',(1.,0.,0.));
#8087=DIRECTION('',(0.,-1.,2.22044604925031E-16));
#8088=DIRECTION('',(1.,0.,0.));
#8089=DIRECTION('',(0.,-1.,2.22044604925031E-16));
#8090=DIRECTION('',(1.,0.,0.));
#8091=DIRECTION('',(0.,-1.,2.22044604925031E-16));
#8092=DIRECTION('',(1.,0.,0.));
#8093=DIRECTION('',(0.,-1.,2.22044604925031E-16));
#8094=DIRECTION('',(1.,0.,0.));
#8095=DIRECTION('',(0.,-1.,2.22044604925031E-16));
#8096=DIRECTION('',(1.,0.,0.));
#8097=DIRECTION('',(0.,-1.,2.22044604925031E-16));
#8098=DIRECTION('',(1.,0.,0.));
#8099=DIRECTION('',(0.,-1.,2.22044604925031E-16));
#8100=DIRECTION('',(1.,0.,0.));
#8101=DIRECTION('',(0.,-1.,2.22044604925031E-16));
#8102=DIRECTION('',(1.,0.,0.));
#8103=DIRECTION('',(0.,-1.,2.22044604925031E-16));
#8104=DIRECTION('',(1.,0.,0.));
#8105=DIRECTION('',(0.,-1.,2.22044604925031E-16));
#8106=DIRECTION('',(1.,0.,0.));
#8107=DIRECTION('axis',(0.,0.,1.));
#8108=DIRECTION('refdir',(1.,0.,0.));
#8109=DIRECTION('axis',(0.,0.,1.));
#8110=DIRECTION('refdir',(1.,0.,0.));
#8111=DIRECTION('center_axis',(0.,0.,1.));
#8112=DIRECTION('ref_axis',(1.,0.,0.));
#8113=DIRECTION('center_axis',(0.,0.,1.));
#8114=DIRECTION('ref_axis',(1.,0.,0.));
#8115=DIRECTION('',(0.,0.,1.));
#8116=DIRECTION('center_axis',(0.,0.,-1.));
#8117=DIRECTION('ref_axis',(1.,0.,0.));
#8118=DIRECTION('center_axis',(0.,0.,1.));
#8119=DIRECTION('ref_axis',(1.,0.,0.));
#8120=DIRECTION('center_axis',(0.,0.,1.));
#8121=DIRECTION('ref_axis',(1.,0.,0.));
#8122=DIRECTION('',(0.,0.,1.));
#8123=DIRECTION('center_axis',(0.,0.,-1.));
#8124=DIRECTION('ref_axis',(1.,0.,0.));
#8125=DIRECTION('center_axis',(0.,0.,1.));
#8126=DIRECTION('ref_axis',(1.,0.,0.));
#8127=DIRECTION('center_axis',(0.,0.,1.));
#8128=DIRECTION('ref_axis',(1.,0.,0.));
#8129=DIRECTION('',(0.,0.,1.));
#8130=DIRECTION('center_axis',(0.,0.,-1.));
#8131=DIRECTION('ref_axis',(1.,0.,0.));
#8132=DIRECTION('center_axis',(0.,0.,1.));
#8133=DIRECTION('ref_axis',(1.,0.,0.));
#8134=DIRECTION('center_axis',(0.,0.,1.));
#8135=DIRECTION('ref_axis',(1.,0.,0.));
#8136=DIRECTION('',(0.,0.,1.));
#8137=DIRECTION('center_axis',(0.,0.,-1.));
#8138=DIRECTION('ref_axis',(1.,0.,0.));
#8139=DIRECTION('center_axis',(0.,0.,1.));
#8140=DIRECTION('ref_axis',(1.,0.,0.));
#8141=DIRECTION('center_axis',(0.,0.,1.));
#8142=DIRECTION('ref_axis',(1.,0.,0.));
#8143=DIRECTION('',(0.,0.,-1.));
#8144=DIRECTION('center_axis',(0.,0.,-1.));
#8145=DIRECTION('ref_axis',(1.,0.,0.));
#8146=DIRECTION('',(0.,0.,1.));
#8147=DIRECTION('center_axis',(0.,0.,1.));
#8148=DIRECTION('ref_axis',(1.,0.,0.));
#8149=DIRECTION('center_axis',(0.,0.,1.));
#8150=DIRECTION('ref_axis',(1.,0.,0.));
#8151=DIRECTION('',(0.,0.,-1.));
#8152=DIRECTION('center_axis',(0.,0.,-1.));
#8153=DIRECTION('ref_axis',(1.,0.,0.));
#8154=DIRECTION('',(0.,0.,1.));
#8155=DIRECTION('center_axis',(0.,0.,1.));
#8156=DIRECTION('ref_axis',(1.,0.,0.));
#8157=DIRECTION('center_axis',(0.,0.,1.));
#8158=DIRECTION('ref_axis',(1.,0.,0.));
#8159=DIRECTION('',(0.,0.,-1.));
#8160=DIRECTION('center_axis',(0.,0.,-1.));
#8161=DIRECTION('ref_axis',(1.,0.,0.));
#8162=DIRECTION('',(0.,0.,1.));
#8163=DIRECTION('center_axis',(0.,0.,1.));
#8164=DIRECTION('ref_axis',(1.,0.,0.));
#8165=DIRECTION('',(0.,0.,-1.));
#8166=DIRECTION('center_axis',(0.,0.,-1.));
#8167=DIRECTION('ref_axis',(1.,0.,0.));
#8168=DIRECTION('',(0.,0.,1.));
#8169=DIRECTION('center_axis',(0.,0.,1.));
#8170=DIRECTION('ref_axis',(1.,0.,0.));
#8171=DIRECTION('center_axis',(0.,0.,1.));
#8172=DIRECTION('ref_axis',(1.,0.,0.));
#8173=DIRECTION('center_axis',(0.,0.,1.));
#8174=DIRECTION('ref_axis',(1.,0.,0.));
#8175=DIRECTION('',(0.,0.,1.));
#8176=DIRECTION('center_axis',(0.,0.,1.));
#8177=DIRECTION('ref_axis',(1.,0.,0.));
#8178=DIRECTION('center_axis',(0.,0.,1.));
#8179=DIRECTION('ref_axis',(1.,0.,0.));
#8180=DIRECTION('center_axis',(0.,0.,1.));
#8181=DIRECTION('ref_axis',(1.,0.,0.));
#8182=DIRECTION('',(0.,0.,1.));
#8183=DIRECTION('center_axis',(0.,0.,1.));
#8184=DIRECTION('ref_axis',(1.,0.,0.));
#8185=DIRECTION('center_axis',(0.,0.,1.));
#8186=DIRECTION('ref_axis',(1.,0.,0.));
#8187=DIRECTION('center_axis',(0.,0.,1.));
#8188=DIRECTION('ref_axis',(1.,0.,0.));
#8189=DIRECTION('',(0.,0.,1.));
#8190=DIRECTION('center_axis',(0.,0.,1.));
#8191=DIRECTION('ref_axis',(1.,0.,0.));
#8192=DIRECTION('center_axis',(0.,0.,1.));
#8193=DIRECTION('ref_axis',(1.,0.,0.));
#8194=DIRECTION('',(0.,1.,0.));
#8195=DIRECTION('',(1.,0.,0.));
#8196=DIRECTION('',(1.70803542250024E-16,1.,0.));
#8197=DIRECTION('center_axis',(0.,0.,-1.));
#8198=DIRECTION('ref_axis',(1.,0.,0.));
#8199=DIRECTION('',(-3.41607084500048E-16,-1.,0.));
#8200=DIRECTION('',(1.,0.,0.));
#8201=DIRECTION('',(0.,-1.,0.));
#8202=DIRECTION('center_axis',(0.,0.,1.));
#8203=DIRECTION('ref_axis',(1.,0.,0.));
#8204=DIRECTION('center_axis',(0.,0.,1.));
#8205=DIRECTION('ref_axis',(1.,0.,0.));
#8206=DIRECTION('',(-1.,0.,0.));
#8207=DIRECTION('',(0.,1.,0.));
#8208=DIRECTION('',(-1.,0.,0.));
#8209=DIRECTION('center_axis',(0.,0.,-1.));
#8210=DIRECTION('ref_axis',(1.,0.,0.));
#8211=DIRECTION('',(1.,0.,0.));
#8212=DIRECTION('',(0.,1.,0.));
#8213=DIRECTION('',(1.,0.,0.));
#8214=DIRECTION('center_axis',(0.,0.,1.));
#8215=DIRECTION('ref_axis',(1.,0.,0.));
#8216=DIRECTION('',(0.,-1.,0.));
#8217=DIRECTION('',(-1.,0.,0.));
#8218=DIRECTION('',(0.,-1.,0.));
#8219=DIRECTION('center_axis',(0.,0.,-1.));
#8220=DIRECTION('ref_axis',(1.,0.,0.));
#8221=DIRECTION('',(0.,1.,0.));
#8222=DIRECTION('',(-1.,0.,0.));
#8223=DIRECTION('',(0.,1.,0.));
#8224=DIRECTION('center_axis',(0.,0.,1.));
#8225=DIRECTION('ref_axis',(1.,0.,0.));
#8226=DIRECTION('',(1.,-1.11022302462516E-16,0.));
#8227=DIRECTION('',(0.,-1.,0.));
#8228=DIRECTION('',(1.,-1.06752213906265E-16,0.));
#8229=DIRECTION('center_axis',(0.,0.,-1.));
#8230=DIRECTION('ref_axis',(1.,0.,0.));
#8231=DIRECTION('',(-1.,1.28102656687518E-16,0.));
#8232=DIRECTION('',(0.,-1.,0.));
#8233=DIRECTION('',(-1.,5.55111512312578E-17,0.));
#8234=DIRECTION('center_axis',(0.,0.,1.));
#8235=DIRECTION('ref_axis',(1.,0.,0.));
#8236=DIRECTION('center_axis',(0.,0.,1.));
#8237=DIRECTION('ref_axis',(1.,0.,0.));
#8238=DIRECTION('center_axis',(0.,0.,1.));
#8239=DIRECTION('ref_axis',(1.,0.,0.));
#8240=DIRECTION('',(0.,0.,1.));
#8241=DIRECTION('center_axis',(0.,0.,1.));
#8242=DIRECTION('ref_axis',(1.,0.,0.));
#8243=DIRECTION('',(0.,0.,-1.));
#8244=DIRECTION('center_axis',(0.,0.,1.));
#8245=DIRECTION('ref_axis',(1.,0.,0.));
#8246=DIRECTION('center_axis',(1.,0.,0.));
#8247=DIRECTION('ref_axis',(0.,1.,0.));
#8248=DIRECTION('',(0.,0.,1.));
#8249=DIRECTION('',(0.,1.,0.));
#8250=DIRECTION('center_axis',(0.,1.,0.));
#8251=DIRECTION('ref_axis',(-1.,0.,0.));
#8252=DIRECTION('',(0.,0.,1.));
#8253=DIRECTION('',(-1.,0.,0.));
#8254=DIRECTION('center_axis',(0.,1.,0.));
#8255=DIRECTION('ref_axis',(-1.,0.,0.));
#8256=DIRECTION('',(0.,0.,1.));
#8257=DIRECTION('',(-1.,0.,0.));
#8258=DIRECTION('',(0.,0.,-1.));
#8259=DIRECTION('center_axis',(-1.,0.,0.));
#8260=DIRECTION('ref_axis',(0.,-1.,0.));
#8261=DIRECTION('',(0.,-1.,0.));
#8262=DIRECTION('center_axis',(-1.,1.70803542250024E-16,0.));
#8263=DIRECTION('ref_axis',(-1.70803542250024E-16,-1.,0.));
#8264=DIRECTION('',(-1.70803542250024E-16,-1.,0.));
#8265=DIRECTION('',(0.,0.,1.));
#8266=DIRECTION('center_axis',(0.,0.,1.));
#8267=DIRECTION('ref_axis',(1.,0.,0.));
#8268=DIRECTION('center_axis',(0.,0.,1.));
#8269=DIRECTION('ref_axis',(1.,0.,0.));
#8270=DIRECTION('',(1.,-5.55111512312578E-17,0.));
#8271=DIRECTION('',(0.,1.,0.));
#8272=DIRECTION('',(1.,-1.28102656687518E-16,0.));
#8273=DIRECTION('center_axis',(0.,0.,1.));
#8274=DIRECTION('ref_axis',(1.,0.,0.));
#8275=DIRECTION('center_axis',(0.,0.,1.));
#8276=DIRECTION('ref_axis',(1.,0.,0.));
#8277=DIRECTION('center_axis',(0.,0.,1.));
#8278=DIRECTION('ref_axis',(1.,0.,0.));
#8279=DIRECTION('center_axis',(0.,0.,1.));
#8280=DIRECTION('ref_axis',(1.,0.,0.));
#8281=DIRECTION('',(3.41607084500048E-16,1.,0.));
#8282=DIRECTION('center_axis',(0.,0.,1.));
#8283=DIRECTION('ref_axis',(1.,0.,0.));
#8284=DIRECTION('center_axis',(0.,0.,1.));
#8285=DIRECTION('ref_axis',(1.,0.,0.));
#8286=DIRECTION('center_axis',(0.,0.,1.));
#8287=DIRECTION('ref_axis',(1.,0.,0.));
#8288=DIRECTION('',(1.,0.,0.));
#8289=DIRECTION('',(0.,-1.,0.));
#8290=DIRECTION('',(1.,0.,0.));
#8291=DIRECTION('center_axis',(0.,0.,1.));
#8292=DIRECTION('ref_axis',(1.,0.,0.));
#8293=DIRECTION('center_axis',(0.,0.,-1.));
#8294=DIRECTION('ref_axis',(1.,0.,0.));
#8295=DIRECTION('center_axis',(0.,0.,1.));
#8296=DIRECTION('ref_axis',(1.,0.,0.));
#8297=DIRECTION('center_axis',(0.,0.,1.));
#8298=DIRECTION('ref_axis',(1.,0.,0.));
#8299=DIRECTION('',(0.,0.,-1.));
#8300=DIRECTION('',(0.,0.,1.));
#8301=DIRECTION('',(0.,0.,1.));
#8302=DIRECTION('center_axis',(0.,0.,1.));
#8303=DIRECTION('ref_axis',(1.,0.,0.));
#8304=DIRECTION('',(0.,0.,-1.));
#8305=DIRECTION('center_axis',(0.,0.,-1.));
#8306=DIRECTION('ref_axis',(1.,0.,0.));
#8307=DIRECTION('',(0.,0.,-1.));
#8308=DIRECTION('center_axis',(0.,0.,1.));
#8309=DIRECTION('ref_axis',(1.,0.,0.));
#8310=DIRECTION('center_axis',(0.,0.,-1.));
#8311=DIRECTION('ref_axis',(1.,0.,0.));
#8312=DIRECTION('',(0.,0.,1.));
#8313=DIRECTION('center_axis',(0.,0.,1.));
#8314=DIRECTION('ref_axis',(1.,0.,0.));
#8315=DIRECTION('',(0.,0.,-1.));
#8316=DIRECTION('center_axis',(0.,0.,-1.));
#8317=DIRECTION('ref_axis',(1.,0.,0.));
#8318=DIRECTION('',(0.,0.,1.));
#8319=DIRECTION('center_axis',(0.,0.,1.));
#8320=DIRECTION('ref_axis',(1.,0.,0.));
#8321=DIRECTION('',(0.,0.,-1.));
#8322=DIRECTION('center_axis',(0.,0.,-1.));
#8323=DIRECTION('ref_axis',(1.,0.,0.));
#8324=DIRECTION('',(0.,0.,1.));
#8325=DIRECTION('center_axis',(1.,-3.41607084500048E-16,0.));
#8326=DIRECTION('ref_axis',(3.41607084500048E-16,1.,0.));
#8327=DIRECTION('center_axis',(0.,0.,1.));
#8328=DIRECTION('ref_axis',(1.,0.,0.));
#8329=DIRECTION('',(0.,0.,-1.));
#8330=DIRECTION('center_axis',(-5.55111512312578E-17,-1.,0.));
#8331=DIRECTION('ref_axis',(1.,-5.55111512312578E-17,0.));
#8332=DIRECTION('',(0.,0.,1.));
#8333=DIRECTION('center_axis',(1.,0.,0.));
#8334=DIRECTION('ref_axis',(0.,1.,0.));
#8335=DIRECTION('',(0.,0.,1.));
#8336=DIRECTION('center_axis',(1.,0.,0.));
#8337=DIRECTION('ref_axis',(0.,1.,0.));
#8338=DIRECTION('',(0.,0.,1.));
#8339=DIRECTION('',(0.,1.,0.));
#8340=DIRECTION('',(0.,0.,-1.));
#8341=DIRECTION('center_axis',(1.11022302462516E-16,1.,0.));
#8342=DIRECTION('ref_axis',(-1.,1.11022302462516E-16,0.));
#8343=DIRECTION('',(-1.,1.11022302462516E-16,0.));
#8344=DIRECTION('center_axis',(1.06752213906265E-16,1.,0.));
#8345=DIRECTION('ref_axis',(-1.,1.06752213906265E-16,0.));
#8346=DIRECTION('',(-1.,1.06752213906265E-16,0.));
#8347=DIRECTION('',(0.,0.,1.));
#8348=DIRECTION('center_axis',(0.,0.,1.));
#8349=DIRECTION('ref_axis',(1.,0.,0.));
#8350=DIRECTION('center_axis',(0.,0.,1.));
#8351=DIRECTION('ref_axis',(1.,0.,0.));
#8352=DIRECTION('',(0.,-1.,0.));
#8353=DIRECTION('',(1.,0.,0.));
#8354=DIRECTION('',(0.,-1.,0.));
#8355=DIRECTION('center_axis',(0.,0.,1.));
#8356=DIRECTION('ref_axis',(1.,0.,0.));
#8357=DIRECTION('center_axis',(0.,0.,1.));
#8358=DIRECTION('ref_axis',(1.,0.,0.));
#8359=DIRECTION('center_axis',(0.,0.,1.));
#8360=DIRECTION('ref_axis',(1.,0.,0.));
#8361=DIRECTION('center_axis',(0.,0.,1.));
#8362=DIRECTION('ref_axis',(1.,0.,0.));
#8363=DIRECTION('center_axis',(0.,0.,1.));
#8364=DIRECTION('ref_axis',(1.,0.,0.));
#8365=DIRECTION('',(0.,0.,1.));
#8366=DIRECTION('center_axis',(-1.28102656687518E-16,-1.,0.));
#8367=DIRECTION('ref_axis',(1.,-1.28102656687518E-16,0.));
#8368=DIRECTION('center_axis',(0.,0.,1.));
#8369=DIRECTION('ref_axis',(1.,0.,0.));
#8370=DIRECTION('',(0.,0.,-1.));
#8371=DIRECTION('center_axis',(-1.,0.,0.));
#8372=DIRECTION('ref_axis',(0.,-1.,0.));
#8373=DIRECTION('',(0.,0.,1.));
#8374=DIRECTION('center_axis',(0.,-1.,0.));
#8375=DIRECTION('ref_axis',(1.,0.,0.));
#8376=DIRECTION('',(0.,0.,1.));
#8377=DIRECTION('center_axis',(0.,-1.,0.));
#8378=DIRECTION('ref_axis',(1.,0.,0.));
#8379=DIRECTION('',(0.,0.,1.));
#8380=DIRECTION('',(1.,0.,0.));
#8381=DIRECTION('',(0.,0.,-1.));
#8382=DIRECTION('center_axis',(1.,0.,0.));
#8383=DIRECTION('ref_axis',(0.,1.,0.));
#8384=DIRECTION('',(0.,1.,0.));
#8385=DIRECTION('center_axis',(1.,0.,0.));
#8386=DIRECTION('ref_axis',(0.,1.,0.));
#8387=DIRECTION('',(0.,1.,0.));
#8388=DIRECTION('',(0.,0.,1.));
#8389=DIRECTION('center_axis',(0.,0.,1.));
#8390=DIRECTION('ref_axis',(1.,0.,0.));
#8391=DIRECTION('center_axis',(0.,0.,1.));
#8392=DIRECTION('ref_axis',(1.,0.,0.));
#8393=DIRECTION('',(-1.,0.,0.));
#8394=DIRECTION('',(0.,-1.,0.));
#8395=DIRECTION('',(-1.,0.,0.));
#8396=DIRECTION('center_axis',(0.,0.,1.));
#8397=DIRECTION('ref_axis',(1.,0.,0.));
#8398=DIRECTION('center_axis',(0.,0.,1.));
#8399=DIRECTION('ref_axis',(1.,0.,0.));
#8400=DIRECTION('center_axis',(0.,0.,1.));
#8401=DIRECTION('ref_axis',(1.,0.,0.));
#8402=DIRECTION('center_axis',(0.,0.,1.));
#8403=DIRECTION('ref_axis',(1.,0.,0.));
#8404=DIRECTION('center_axis',(0.,0.,1.));
#8405=DIRECTION('ref_axis',(1.,0.,0.));
#8406=DIRECTION('',(0.,0.,1.));
#8407=DIRECTION('center_axis',(-1.,0.,0.));
#8408=DIRECTION('ref_axis',(0.,-1.,0.));
#8409=DIRECTION('center_axis',(0.,0.,1.));
#8410=DIRECTION('ref_axis',(1.,0.,0.));
#8411=DIRECTION('',(0.,0.,-1.));
#8412=DIRECTION('center_axis',(0.,1.,0.));
#8413=DIRECTION('ref_axis',(-1.,0.,0.));
#8414=DIRECTION('',(0.,0.,1.));
#8415=DIRECTION('center_axis',(0.,-1.,0.));
#8416=DIRECTION('ref_axis',(1.,0.,0.));
#8417=DIRECTION('',(0.,0.,1.));
#8418=DIRECTION('center_axis',(-1.,0.,0.));
#8419=DIRECTION('ref_axis',(0.,-1.,0.));
#8420=DIRECTION('',(0.,0.,-1.));
#8421=DIRECTION('center_axis',(-1.,0.,0.));
#8422=DIRECTION('ref_axis',(0.,-1.,0.));
#8423=DIRECTION('',(0.,0.,1.));
#8424=DIRECTION('center_axis',(0.,0.,1.));
#8425=DIRECTION('ref_axis',(1.,0.,0.));
#8426=DIRECTION('center_axis',(0.,0.,1.));
#8427=DIRECTION('ref_axis',(1.,0.,0.));
#8428=DIRECTION('center_axis',(0.,0.,1.));
#8429=DIRECTION('ref_axis',(-1.,1.22464679914735E-16,0.));
#8430=DIRECTION('',(0.,0.,1.));
#8431=DIRECTION('',(0.,0.,1.));
#8432=DIRECTION('center_axis',(0.,1.,0.));
#8433=DIRECTION('ref_axis',(-1.,0.,0.));
#8434=DIRECTION('center_axis',(0.,-1.,0.));
#8435=DIRECTION('ref_axis',(1.,0.,0.));
#8436=DIRECTION('center_axis',(0.,0.,1.));
#8437=DIRECTION('ref_axis',(1.,0.,0.));
#8438=DIRECTION('center_axis',(0.,0.,-1.));
#8439=DIRECTION('ref_axis',(1.,0.,0.));
#8440=DIRECTION('center_axis',(0.,0.,1.));
#8441=DIRECTION('ref_axis',(1.,0.,0.));
#8442=DIRECTION('',(0.,0.,-1.));
#8443=DIRECTION('center_axis',(0.,0.,1.));
#8444=DIRECTION('ref_axis',(1.,0.,0.));
#8445=DIRECTION('center_axis',(0.,0.,1.));
#8446=DIRECTION('ref_axis',(1.,0.,0.));
#8447=DIRECTION('axis',(0.,0.,1.));
#8448=DIRECTION('refdir',(1.,0.,0.));
#8449=DIRECTION('center_axis',(0.,0.,1.));
#8450=DIRECTION('ref_axis',(1.,0.,0.));
#8451=DIRECTION('center_axis',(0.,0.,-1.));
#8452=DIRECTION('ref_axis',(1.,0.,0.));
#8453=DIRECTION('',(0.,0.,-1.));
#8454=DIRECTION('center_axis',(0.,0.,-1.));
#8455=DIRECTION('ref_axis',(1.,0.,0.));
#8456=DIRECTION('center_axis',(0.,0.,1.));
#8457=DIRECTION('ref_axis',(1.,0.,0.));
#8458=DIRECTION('center_axis',(0.,0.,1.));
#8459=DIRECTION('ref_axis',(1.,0.,0.));
#8460=DIRECTION('',(0.,0.,-1.));
#8461=DIRECTION('center_axis',(0.,0.,1.));
#8462=DIRECTION('ref_axis',(1.,0.,0.));
#8463=DIRECTION('center_axis',(0.,0.,1.));
#8464=DIRECTION('ref_axis',(1.,0.,0.));
#8465=DIRECTION('center_axis',(0.,0.,1.));
#8466=DIRECTION('ref_axis',(1.,0.,0.));
#8467=DIRECTION('axis',(0.,0.,1.));
#8468=DIRECTION('refdir',(1.,0.,0.));
#8469=DIRECTION('center_axis',(0.,1.,0.));
#8470=DIRECTION('ref_axis',(1.,0.,0.));
#8471=DIRECTION('',(0.,0.,-1.));
#8472=DIRECTION('center_axis',(0.,1.,0.));
#8473=DIRECTION('ref_axis',(1.,0.,0.));
#8474=DIRECTION('center_axis',(0.,1.,0.));
#8475=DIRECTION('ref_axis',(1.,0.,0.));
#8476=DIRECTION('center_axis',(0.,1.,0.));
#8477=DIRECTION('ref_axis',(1.,0.,0.));
#8478=DIRECTION('',(0.,1.,0.));
#8479=DIRECTION('center_axis',(0.,1.,0.));
#8480=DIRECTION('ref_axis',(1.,0.,0.));
#8481=DIRECTION('center_axis',(0.,1.,0.));
#8482=DIRECTION('ref_axis',(1.,0.,0.));
#8483=DIRECTION('',(0.,0.,1.));
#8484=DIRECTION('center_axis',(1.,0.,0.));
#8485=DIRECTION('ref_axis',(0.,0.,-1.));
#8486=DIRECTION('',(0.,0.,-1.));
#8487=DIRECTION('center_axis',(1.,0.,0.));
#8488=DIRECTION('ref_axis',(0.,0.,-1.));
#8489=DIRECTION('center_axis',(1.,0.,0.));
#8490=DIRECTION('ref_axis',(0.,0.,-1.));
#8491=DIRECTION('',(1.,0.,0.));
#8492=DIRECTION('center_axis',(1.,0.,0.));
#8493=DIRECTION('ref_axis',(0.,0.,-1.));
#8494=DIRECTION('center_axis',(1.,0.,0.));
#8495=DIRECTION('ref_axis',(0.,0.,-1.));
#8496=DIRECTION('',(0.,0.,1.));
#8497=DIRECTION('center_axis',(0.,0.,1.));
#8498=DIRECTION('ref_axis',(1.,0.,0.));
#8499=DIRECTION('center_axis',(0.,0.,-1.));
#8500=DIRECTION('ref_axis',(1.,0.,0.));
#8501=DIRECTION('',(0.,0.,-1.));
#8502=DIRECTION('',(0.,0.,-1.));
#8503=DIRECTION('center_axis',(0.,0.,-1.));
#8504=DIRECTION('ref_axis',(1.,0.,0.));
#8505=DIRECTION('center_axis',(0.,0.,1.));
#8506=DIRECTION('ref_axis',(1.,0.,0.));
#8507=DIRECTION('center_axis',(0.,0.,1.));
#8508=DIRECTION('ref_axis',(1.,0.,0.));
#8509=DIRECTION('',(0.,0.,-1.));
#8510=DIRECTION('',(0.,0.,-1.));
#8511=DIRECTION('center_axis',(0.,0.,1.));
#8512=DIRECTION('ref_axis',(1.,0.,0.));
#8513=DIRECTION('center_axis',(0.,0.,1.));
#8514=DIRECTION('ref_axis',(1.,0.,0.));
#8515=DIRECTION('center_axis',(0.,0.,1.));
#8516=DIRECTION('ref_axis',(1.,0.,0.));
#8517=DIRECTION('axis',(0.,0.,1.));
#8518=DIRECTION('refdir',(1.,0.,0.));
#8519=DIRECTION('center_axis',(0.,1.,0.));
#8520=DIRECTION('ref_axis',(1.,0.,0.));
#8521=DIRECTION('center_axis',(0.,1.,0.));
#8522=DIRECTION('ref_axis',(1.,0.,0.));
#8523=DIRECTION('center_axis',(0.866025403784439,0.,-0.5));
#8524=DIRECTION('ref_axis',(0.5,0.,0.866025403784439));
#8525=DIRECTION('',(0.5,0.,0.866025403784439));
#8526=DIRECTION('',(0.,-1.,0.));
#8527=DIRECTION('',(0.5,0.,0.866025403784439));
#8528=DIRECTION('',(0.,-1.,0.));
#8529=DIRECTION('center_axis',(1.20185167898973E-16,0.,-1.));
#8530=DIRECTION('ref_axis',(1.,0.,1.20185167898973E-16));
#8531=DIRECTION('',(1.,0.,1.20185167898973E-16));
#8532=DIRECTION('',(0.,-1.,0.));
#8533=DIRECTION('',(1.,0.,1.20185167898973E-16));
#8534=DIRECTION('center_axis',(-0.866025403784439,0.,-0.5));
#8535=DIRECTION('ref_axis',(0.5,0.,-0.866025403784439));
#8536=DIRECTION('',(0.5,0.,-0.866025403784439));
#8537=DIRECTION('',(0.,-1.,0.));
#8538=DIRECTION('',(0.5,0.,-0.866025403784439));
#8539=DIRECTION('center_axis',(-0.866025403784439,0.,0.5));
#8540=DIRECTION('ref_axis',(-0.5,0.,-0.866025403784439));
#8541=DIRECTION('',(-0.5,0.,-0.866025403784439));
#8542=DIRECTION('',(0.,-1.,0.));
#8543=DIRECTION('',(-0.5,0.,-0.866025403784439));
#8544=DIRECTION('center_axis',(-2.40370335797945E-16,0.,1.));
#8545=DIRECTION('ref_axis',(-1.,0.,-2.40370335797945E-16));
#8546=DIRECTION('',(-1.,0.,-2.40370335797945E-16));
#8547=DIRECTION('',(0.,-1.,0.));
#8548=DIRECTION('',(-1.,0.,-2.40370335797945E-16));
#8549=DIRECTION('center_axis',(0.866025403784439,0.,0.5));
#8550=DIRECTION('ref_axis',(-0.5,0.,0.866025403784439));
#8551=DIRECTION('',(-0.5,0.,0.866025403784439));
#8552=DIRECTION('',(-0.5,0.,0.866025403784439));
#8553=DIRECTION('center_axis',(0.,-1.,0.));
#8554=DIRECTION('ref_axis',(0.,0.,-1.));
#8555=DIRECTION('center_axis',(0.,1.,0.));
#8556=DIRECTION('ref_axis',(0.,0.,1.));
#8557=DIRECTION('center_axis',(0.,-1.,0.));
#8558=DIRECTION('ref_axis',(1.,0.,0.));
#8559=DIRECTION('center_axis',(0.,-1.,0.));
#8560=DIRECTION('ref_axis',(1.,0.,0.));
#8561=DIRECTION('center_axis',(0.,-1.,0.));
#8562=DIRECTION('ref_axis',(1.,0.,0.));
#8563=DIRECTION('',(0.707106781186548,0.707106781186547,8.65956056235494E-17));
#8564=DIRECTION('center_axis',(0.,-1.,0.));
#8565=DIRECTION('ref_axis',(1.,0.,0.));
#8566=DIRECTION('',(0.,1.,0.));
#8567=DIRECTION('',(0.,0.,1.));
#8568=DIRECTION('',(1.,0.,0.));
#8569=DIRECTION('',(0.,0.,1.));
#8570=DIRECTION('',(1.,0.,0.));
#8571=DIRECTION('',(0.,0.,1.));
#8572=DIRECTION('',(1.,0.,0.));
#8573=DIRECTION('',(0.,0.,1.));
#8574=DIRECTION('',(1.,0.,0.));
#8575=DIRECTION('',(0.,0.,1.));
#8576=DIRECTION('',(1.,0.,0.));
#8577=DIRECTION('',(0.,0.,1.));
#8578=DIRECTION('',(1.,0.,0.));
#8579=DIRECTION('',(0.,0.,1.));
#8580=DIRECTION('',(1.,0.,0.));
#8581=DIRECTION('',(0.,0.,1.));
#8582=DIRECTION('',(1.,0.,0.));
#8583=DIRECTION('',(0.,0.,1.));
#8584=DIRECTION('',(-1.,1.22464679914735E-16,0.));
#8585=DIRECTION('',(0.,-1.,2.22044604925031E-16));
#8586=DIRECTION('',(1.,0.,0.));
#8587=DIRECTION('',(0.,0.,1.));
#8588=DIRECTION('',(1.,0.,0.));
#8589=DIRECTION('',(0.,0.,1.));
#8590=DIRECTION('',(1.,0.,0.));
#8591=DIRECTION('',(0.,0.,1.));
#8592=DIRECTION('',(1.,0.,0.));
#8593=DIRECTION('',(0.,0.,1.));
#8594=DIRECTION('',(-1.,1.22464679914735E-16,0.));
#8595=DIRECTION('',(0.,0.,1.));
#8596=DIRECTION('',(1.,0.,0.));
#8597=DIRECTION('',(0.,0.,1.));
#8598=DIRECTION('',(1.,0.,0.));
#8599=DIRECTION('',(0.,0.,1.));
#8600=DIRECTION('',(1.,0.,0.));
#8601=CARTESIAN_POINT('',(0.,0.,0.));
#8602=CARTESIAN_POINT('',(0.,0.,0.));
#8603=CARTESIAN_POINT('',(0.,0.,0.));
#8604=CARTESIAN_POINT('Origin',(5.94264068711928,-1.7,-0.1));
#8605=CARTESIAN_POINT('',(5.73264068711928,-1.7,0.));
#8606=CARTESIAN_POINT('Origin',(5.94264068711928,-1.7,0.));
#8607=CARTESIAN_POINT('',(5.73264068711928,-1.7,1.));
#8608=CARTESIAN_POINT('',(5.73264068711928,-1.7,-0.1));
#8609=CARTESIAN_POINT('Origin',(5.94264068711928,-1.7,1.));
#8610=CARTESIAN_POINT('Origin',(-1.7,1.7,-0.1));
#8611=CARTESIAN_POINT('',(-1.91,1.7,0.));
#8612=CARTESIAN_POINT('Origin',(-1.7,1.7,0.));
#8613=CARTESIAN_POINT('',(-1.91,1.7,1.));
#8614=CARTESIAN_POINT('',(-1.91,1.7,-0.1));
#8615=CARTESIAN_POINT('Origin',(-1.7,1.7,1.));
#8616=CARTESIAN_POINT('Origin',(-1.7,-1.7,-0.1));
#8617=CARTESIAN_POINT('',(-1.91,-1.7,0.));
#8618=CARTESIAN_POINT('Origin',(-1.7,-1.7,0.));
#8619=CARTESIAN_POINT('',(-1.91,-1.7,1.));
#8620=CARTESIAN_POINT('',(-1.91,-1.7,-0.1));
#8621=CARTESIAN_POINT('Origin',(-1.7,-1.7,1.));
#8622=CARTESIAN_POINT('Origin',(5.94264068711928,1.7,-0.1));
#8623=CARTESIAN_POINT('',(5.73264068711928,1.7,0.));
#8624=CARTESIAN_POINT('Origin',(5.94264068711928,1.7,0.));
#8625=CARTESIAN_POINT('',(5.73264068711928,1.7,1.));
#8626=CARTESIAN_POINT('',(5.73264068711928,1.7,-0.1));
#8627=CARTESIAN_POINT('Origin',(5.94264068711928,1.7,1.));
#8628=CARTESIAN_POINT('Origin',(8.,4.,0.));
#8629=CARTESIAN_POINT('',(8.,4.,0.));
#8630=CARTESIAN_POINT('',(-3.5,4.,0.));
#8631=CARTESIAN_POINT('',(8.,4.,0.));
#8632=CARTESIAN_POINT('',(-3.5,4.,1.));
#8633=CARTESIAN_POINT('',(-3.5,4.,0.));
#8634=CARTESIAN_POINT('',(8.,4.,1.));
#8635=CARTESIAN_POINT('',(8.,4.,1.));
#8636=CARTESIAN_POINT('',(8.,4.,0.));
#8637=CARTESIAN_POINT('Origin',(8.,-4.,0.));
#8638=CARTESIAN_POINT('',(8.,-4.,0.));
#8639=CARTESIAN_POINT('',(8.,-4.,0.));
#8640=CARTESIAN_POINT('',(8.,-4.,1.));
#8641=CARTESIAN_POINT('',(8.,-4.,1.));
#8642=CARTESIAN_POINT('',(8.,-4.,0.));
#8643=CARTESIAN_POINT('Origin',(-3.5,-4.,0.));
#8644=CARTESIAN_POINT('',(-3.5,-4.,0.));
#8645=CARTESIAN_POINT('',(-3.5,-4.,0.));
#8646=CARTESIAN_POINT('',(-3.5,-4.,1.));
#8647=CARTESIAN_POINT('',(-3.5,-4.,1.));
#8648=CARTESIAN_POINT('',(-3.5,-4.,0.));
#8649=CARTESIAN_POINT('Origin',(-3.5,4.,0.));
#8650=CARTESIAN_POINT('',(-3.5,4.,0.));
#8651=CARTESIAN_POINT('',(-3.5,4.,1.));
#8652=CARTESIAN_POINT('Origin',(2.25,0.,1.));
#8653=CARTESIAN_POINT('Origin',(2.25,0.,0.));
#8654=CARTESIAN_POINT('',(0.,0.,0.));
#8655=CARTESIAN_POINT('Origin',(8.,-3.2,-0.6));
#8656=CARTESIAN_POINT('',(8.,-3.2,-0.6));
#8657=CARTESIAN_POINT('',(-3.5,-3.2,-0.6));
#8658=CARTESIAN_POINT('',(8.,-3.2,-0.6));
#8659=CARTESIAN_POINT('',(-3.5,-3.2,0.));
#8660=CARTESIAN_POINT('',(-3.5,-3.2,-0.6));
#8661=CARTESIAN_POINT('',(8.,-3.2,0.));
#8662=CARTESIAN_POINT('',(8.,-3.2,0.));
#8663=CARTESIAN_POINT('',(8.,-3.2,-0.6));
#8664=CARTESIAN_POINT('Origin',(8.,-4.,-0.6));
#8665=CARTESIAN_POINT('',(8.,-4.,-0.6));
#8666=CARTESIAN_POINT('',(8.,-4.,-0.6));
#8667=CARTESIAN_POINT('',(8.,-4.,0.));
#8668=CARTESIAN_POINT('',(8.,-4.,0.));
#8669=CARTESIAN_POINT('',(8.,-4.,-0.6));
#8670=CARTESIAN_POINT('Origin',(-3.5,-4.,-0.6));
#8671=CARTESIAN_POINT('',(-3.5,-4.,-0.6));
#8672=CARTESIAN_POINT('',(-3.5,-4.,-0.6));
#8673=CARTESIAN_POINT('',(-3.5,-4.,0.));
#8674=CARTESIAN_POINT('',(-3.5,-4.,0.));
#8675=CARTESIAN_POINT('',(-3.5,-4.,-0.6));
#8676=CARTESIAN_POINT('Origin',(-3.5,-3.2,-0.6));
#8677=CARTESIAN_POINT('',(-3.5,-3.2,-0.6));
#8678=CARTESIAN_POINT('',(-3.5,-3.2,0.));
#8679=CARTESIAN_POINT('Origin',(2.25,-3.6,0.));
#8680=CARTESIAN_POINT('Origin',(2.25,-3.6,-0.6));
#8681=CARTESIAN_POINT('',(0.,0.,0.));
#8682=CARTESIAN_POINT('Origin',(8.,4.,-0.6));
#8683=CARTESIAN_POINT('',(8.,4.,-0.6));
#8684=CARTESIAN_POINT('',(-3.5,4.,-0.6));
#8685=CARTESIAN_POINT('',(8.,4.,-0.6));
#8686=CARTESIAN_POINT('',(-3.5,4.,0.));
#8687=CARTESIAN_POINT('',(-3.5,4.,-0.6));
#8688=CARTESIAN_POINT('',(8.,4.,0.));
#8689=CARTESIAN_POINT('',(8.,4.,0.));
#8690=CARTESIAN_POINT('',(8.,4.,-0.6));
#8691=CARTESIAN_POINT('Origin',(8.,3.2,-0.6));
#8692=CARTESIAN_POINT('',(8.,3.2,-0.6));
#8693=CARTESIAN_POINT('',(8.,3.2,-0.6));
#8694=CARTESIAN_POINT('',(8.,3.2,0.));
#8695=CARTESIAN_POINT('',(8.,3.2,0.));
#8696=CARTESIAN_POINT('',(8.,3.2,-0.6));
#8697=CARTESIAN_POINT('Origin',(-3.5,3.2,-0.6));
#8698=CARTESIAN_POINT('',(-3.5,3.2,-0.6));
#8699=CARTESIAN_POINT('',(-3.5,3.2,-0.6));
#8700=CARTESIAN_POINT('',(-3.5,3.2,0.));
#8701=CARTESIAN_POINT('',(-3.5,3.2,0.));
#8702=CARTESIAN_POINT('',(-3.5,3.2,-0.6));
#8703=CARTESIAN_POINT('Origin',(-3.5,4.,-0.6));
#8704=CARTESIAN_POINT('',(-3.5,4.,-0.6));
#8705=CARTESIAN_POINT('',(-3.5,4.,0.));
#8706=CARTESIAN_POINT('Origin',(2.25,3.6,0.));
#8707=CARTESIAN_POINT('Origin',(2.25,3.6,-0.6));
#8708=CARTESIAN_POINT('',(0.,0.,0.));
#8709=CARTESIAN_POINT('Origin',(4.24264068711929,-2.3,1.4));
#8710=CARTESIAN_POINT('',(3.99264068711929,-2.2,1.4));
#8711=CARTESIAN_POINT('Origin',(4.24264068711929,-2.2,1.4));
#8712=CARTESIAN_POINT('',(3.99264068711929,-0.988888264668966,1.4));
#8713=CARTESIAN_POINT('',(3.99264068711929,-2.3,1.4));
#8714=CARTESIAN_POINT('Ctrl Pts',(3.99264068711929,-0.988888264668966,1.4));
#8715=CARTESIAN_POINT('Ctrl Pts',(3.99264068711929,-0.988888264668966,1.36846860584118));
#8716=CARTESIAN_POINT('Ctrl Pts',(3.99896863868788,-0.990553370646674,1.33492785033683));
#8717=CARTESIAN_POINT('Ctrl Pts',(4.02452085710491,-0.996491737296663,1.27337379025046));
#8718=CARTESIAN_POINT('Ctrl Pts',(4.04373855891321,-1.00067109353237,1.2453487376128));
#8719=CARTESIAN_POINT('Ctrl Pts',(4.08798657355057,-1.00845756932386,1.20110072297544));
#8720=CARTESIAN_POINT('Ctrl Pts',(4.11601281617403,-1.01258144235289,1.18188079690607));
#8721=CARTESIAN_POINT('Ctrl Pts',(4.17757108672792,-1.0183917429657,1.15632695599232));
#8722=CARTESIAN_POINT('Ctrl Pts',(4.21111335623591,-1.02,1.15));
#8723=CARTESIAN_POINT('Ctrl Pts',(4.27416801800266,-1.02,1.15));
#8724=CARTESIAN_POINT('Ctrl Pts',(4.30771028751065,-1.0183917429657,1.15632695599232));
#8725=CARTESIAN_POINT('Ctrl Pts',(4.36926855806454,-1.01258144235289,1.18188079690607));
#8726=CARTESIAN_POINT('Ctrl Pts',(4.397294800688,-1.00845756932386,1.20110072297544));
#8727=CARTESIAN_POINT('Ctrl Pts',(4.44154281532536,-1.00067109353237,1.2453487376128));
#8728=CARTESIAN_POINT('Ctrl Pts',(4.46076051713366,-0.996491737296663,1.27337379025046));
#8729=CARTESIAN_POINT('Ctrl Pts',(4.48631273555069,-0.990553370646674,1.33492785033683));
#8730=CARTESIAN_POINT('Ctrl Pts',(4.49264068711929,-0.988888264668966,1.36846860584118));
#8731=CARTESIAN_POINT('Ctrl Pts',(4.49264068711929,-0.988888264668966,1.43153139415882));
#8732=CARTESIAN_POINT('Ctrl Pts',(4.48631273555069,-0.990553370646674,1.46507214966317));
#8733=CARTESIAN_POINT('Ctrl Pts',(4.46076051713366,-0.996491737296663,1.52662620974954));
#8734=CARTESIAN_POINT('Ctrl Pts',(4.44154281532536,-1.00067109353237,1.5546512623872));
#8735=CARTESIAN_POINT('Ctrl Pts',(4.397294800688,-1.00845756932386,1.59889927702456));
#8736=CARTESIAN_POINT('Ctrl Pts',(4.36926855806454,-1.01258144235289,1.61811920309393));
#8737=CARTESIAN_POINT('Ctrl Pts',(4.30771028751065,-1.0183917429657,1.64367304400768));
#8738=CARTESIAN_POINT('Ctrl Pts',(4.27416801800266,-1.02,1.65));
#8739=CARTESIAN_POINT('Ctrl Pts',(4.21111335623591,-1.02,1.65));
#8740=CARTESIAN_POINT('Ctrl Pts',(4.17757108672792,-1.0183917429657,1.64367304400768));
#8741=CARTESIAN_POINT('Ctrl Pts',(4.11601281617403,-1.01258144235289,1.61811920309393));
#8742=CARTESIAN_POINT('Ctrl Pts',(4.08798657355057,-1.00845756932386,1.59889927702456));
#8743=CARTESIAN_POINT('Ctrl Pts',(4.04373855891321,-1.00067109353237,1.5546512623872));
#8744=CARTESIAN_POINT('Ctrl Pts',(4.02452085710491,-0.996491737296663,1.52662620974954));
#8745=CARTESIAN_POINT('Ctrl Pts',(3.99896863868788,-0.990553370646674,1.46507214966317));
#8746=CARTESIAN_POINT('Ctrl Pts',(3.99264068711929,-0.988888264668966,1.43153139415882));
#8747=CARTESIAN_POINT('Ctrl Pts',(3.99264068711929,-0.988888264668966,1.4));
#8748=CARTESIAN_POINT('Origin',(2.52264068711929,2.10639249453345E-16,2.9));
#8749=CARTESIAN_POINT('',(2.35764068711929,1.90432577267413E-16,2.9));
#8750=CARTESIAN_POINT('Origin',(2.52264068711929,2.10639249453345E-16,2.9));
#8751=CARTESIAN_POINT('',(2.35764068711929,2.30845921639276E-16,3.6));
#8752=CARTESIAN_POINT('',(2.35764068711929,1.90432577267413E-16,2.9));
#8753=CARTESIAN_POINT('Origin',(2.52264068711929,2.10639249453345E-16,3.6));
#8754=CARTESIAN_POINT('Origin',(2.52264068711929,2.22044604925031E-16,2.9));
#8755=CARTESIAN_POINT('Origin',(4.24264068711929,1.72,2.9));
#8756=CARTESIAN_POINT('',(4.07764068711929,1.72,2.9));
#8757=CARTESIAN_POINT('Origin',(4.24264068711929,1.72,2.9));
#8758=CARTESIAN_POINT('',(4.07764068711929,1.72,3.6));
#8759=CARTESIAN_POINT('',(4.07764068711929,1.72,2.9));
#8760=CARTESIAN_POINT('Origin',(4.24264068711929,1.72,3.6));
#8761=CARTESIAN_POINT('Origin',(4.24264068711929,1.72,2.9));
#8762=CARTESIAN_POINT('Origin',(5.96264068711929,0.,2.9));
#8763=CARTESIAN_POINT('',(5.79764068711929,-2.02066721859313E-17,2.9));
#8764=CARTESIAN_POINT('Origin',(5.96264068711929,0.,2.9));
#8765=CARTESIAN_POINT('',(5.79764068711929,2.02066721859313E-17,3.6));
#8766=CARTESIAN_POINT('',(5.79764068711929,-2.02066721859313E-17,2.9));
#8767=CARTESIAN_POINT('Origin',(5.96264068711929,0.,3.6));
#8768=CARTESIAN_POINT('Origin',(5.96264068711929,0.,2.9));
#8769=CARTESIAN_POINT('Origin',(4.24264068711929,-1.72,2.9));
#8770=CARTESIAN_POINT('',(4.07764068711929,-1.72,2.9));
#8771=CARTESIAN_POINT('Origin',(4.24264068711929,-1.72,2.9));
#8772=CARTESIAN_POINT('',(4.07764068711929,-1.72,3.6));
#8773=CARTESIAN_POINT('',(4.07764068711929,-1.72,2.9));
#8774=CARTESIAN_POINT('Origin',(4.24264068711929,-1.72,3.6));
#8775=CARTESIAN_POINT('Origin',(4.24264068711929,-1.72,2.9));
#8776=CARTESIAN_POINT('Origin',(4.24264068711929,0.,2.05));
#8777=CARTESIAN_POINT('',(2.74264068711929,-1.83697019872103E-16,2.05));
#8778=CARTESIAN_POINT('Origin',(4.24264068711929,0.,2.05));
#8779=CARTESIAN_POINT('',(2.74264068711929,1.83697019872103E-16,3.6));
#8780=CARTESIAN_POINT('',(2.74264068711929,-1.83697019872103E-16,2.05));
#8781=CARTESIAN_POINT('Origin',(4.24264068711929,0.,3.6));
#8782=CARTESIAN_POINT('Origin',(4.24264068711929,0.,2.05));
#8783=CARTESIAN_POINT('',(3.22264068711929,-1.2491397351303E-16,2.05));
#8784=CARTESIAN_POINT('Origin',(4.24264068711929,0.,2.05));
#8785=CARTESIAN_POINT('Origin',(4.24264068711929,0.,0.9));
#8786=CARTESIAN_POINT('',(3.22264068711929,-1.2491397351303E-16,1.));
#8787=CARTESIAN_POINT('Origin',(4.24264068711929,0.,1.));
#8788=CARTESIAN_POINT('',(3.22264068711929,-1.2491397351303E-16,0.9));
#8789=CARTESIAN_POINT('Origin',(0.,-2.3,1.4));
#8790=CARTESIAN_POINT('',(-0.25,-2.2,1.4));
#8791=CARTESIAN_POINT('Origin',(0.,-2.2,1.4));
#8792=CARTESIAN_POINT('',(-0.25,-0.988888264668967,1.4));
#8793=CARTESIAN_POINT('',(-0.25,-2.3,1.4));
#8794=CARTESIAN_POINT('Ctrl Pts',(-0.25,-0.988888264668967,1.4));
#8795=CARTESIAN_POINT('Ctrl Pts',(-0.25,-0.988888264668967,1.36846860584118));
#8796=CARTESIAN_POINT('Ctrl Pts',(-0.243672048431404,-0.990553370646674,
1.33492785033683));
#8797=CARTESIAN_POINT('Ctrl Pts',(-0.218119830014375,-0.996491737296663,
1.27337379025046));
#8798=CARTESIAN_POINT('Ctrl Pts',(-0.198902128206072,-1.00067109353237,
1.2453487376128));
#8799=CARTESIAN_POINT('Ctrl Pts',(-0.154654113568716,-1.00845756932386,
1.20110072297544));
#8800=CARTESIAN_POINT('Ctrl Pts',(-0.126627870945253,-1.01258144235289,
1.18188079690607));
#8801=CARTESIAN_POINT('Ctrl Pts',(-0.0650696003913631,-1.0183917429657,
1.15632695599232));
#8802=CARTESIAN_POINT('Ctrl Pts',(-0.031527330883376,-1.02,1.15));
#8803=CARTESIAN_POINT('Ctrl Pts',(0.031527330883376,-1.02,1.15));
#8804=CARTESIAN_POINT('Ctrl Pts',(0.065069600391363,-1.0183917429657,1.15632695599232));
#8805=CARTESIAN_POINT('Ctrl Pts',(0.126627870945253,-1.01258144235289,1.18188079690607));
#8806=CARTESIAN_POINT('Ctrl Pts',(0.154654113568716,-1.00845756932386,1.20110072297544));
#8807=CARTESIAN_POINT('Ctrl Pts',(0.198902128206072,-1.00067109353237,1.2453487376128));
#8808=CARTESIAN_POINT('Ctrl Pts',(0.218119830014375,-0.996491737296663,
1.27337379025046));
#8809=CARTESIAN_POINT('Ctrl Pts',(0.243672048431404,-0.990553370646674,
1.33492785033683));
#8810=CARTESIAN_POINT('Ctrl Pts',(0.25,-0.988888264668967,1.36846860584118));
#8811=CARTESIAN_POINT('Ctrl Pts',(0.25,-0.988888264668967,1.43153139415882));
#8812=CARTESIAN_POINT('Ctrl Pts',(0.243672048431404,-0.990553370646674,
1.46507214966317));
#8813=CARTESIAN_POINT('Ctrl Pts',(0.218119830014375,-0.996491737296663,
1.52662620974954));
#8814=CARTESIAN_POINT('Ctrl Pts',(0.198902128206072,-1.00067109353237,1.5546512623872));
#8815=CARTESIAN_POINT('Ctrl Pts',(0.154654113568716,-1.00845756932386,1.59889927702456));
#8816=CARTESIAN_POINT('Ctrl Pts',(0.126627870945253,-1.01258144235289,1.61811920309393));
#8817=CARTESIAN_POINT('Ctrl Pts',(0.065069600391363,-1.0183917429657,1.64367304400768));
#8818=CARTESIAN_POINT('Ctrl Pts',(0.031527330883376,-1.02,1.65));
#8819=CARTESIAN_POINT('Ctrl Pts',(-0.031527330883376,-1.02,1.65));
#8820=CARTESIAN_POINT('Ctrl Pts',(-0.065069600391363,-1.0183917429657,1.64367304400768));
#8821=CARTESIAN_POINT('Ctrl Pts',(-0.126627870945253,-1.01258144235289,
1.61811920309393));
#8822=CARTESIAN_POINT('Ctrl Pts',(-0.154654113568716,-1.00845756932386,
1.59889927702456));
#8823=CARTESIAN_POINT('Ctrl Pts',(-0.198902128206072,-1.00067109353237,
1.5546512623872));
#8824=CARTESIAN_POINT('Ctrl Pts',(-0.218119830014375,-0.996491737296663,
1.52662620974954));
#8825=CARTESIAN_POINT('Ctrl Pts',(-0.243672048431404,-0.990553370646674,
1.46507214966317));
#8826=CARTESIAN_POINT('Ctrl Pts',(-0.25,-0.988888264668966,1.43153139415882));
#8827=CARTESIAN_POINT('Ctrl Pts',(-0.25,-0.988888264668966,1.4));
#8828=CARTESIAN_POINT('Origin',(-1.72,2.10639249453345E-16,2.9));
#8829=CARTESIAN_POINT('',(-1.885,1.90432577267413E-16,2.9));
#8830=CARTESIAN_POINT('Origin',(-1.72,2.10639249453345E-16,2.9));
#8831=CARTESIAN_POINT('',(-1.885,2.30845921639276E-16,3.6));
#8832=CARTESIAN_POINT('',(-1.885,1.90432577267413E-16,2.9));
#8833=CARTESIAN_POINT('Origin',(-1.72,2.10639249453345E-16,3.6));
#8834=CARTESIAN_POINT('Origin',(-1.72,2.22044604925031E-16,2.9));
#8835=CARTESIAN_POINT('Origin',(1.05319624726672E-16,1.72,2.9));
#8836=CARTESIAN_POINT('',(-0.165,1.72,2.9));
#8837=CARTESIAN_POINT('Origin',(1.05319624726672E-16,1.72,2.9));
#8838=CARTESIAN_POINT('',(-0.165,1.72,3.6));
#8839=CARTESIAN_POINT('',(-0.165,1.72,2.9));
#8840=CARTESIAN_POINT('Origin',(1.05319624726672E-16,1.72,3.6));
#8841=CARTESIAN_POINT('Origin',(1.11022302462516E-16,1.72,2.9));
#8842=CARTESIAN_POINT('Origin',(1.72,0.,2.9));
#8843=CARTESIAN_POINT('',(1.555,-2.02066721859313E-17,2.9));
#8844=CARTESIAN_POINT('Origin',(1.72,0.,2.9));
#8845=CARTESIAN_POINT('',(1.555,2.02066721859313E-17,3.6));
#8846=CARTESIAN_POINT('',(1.555,-2.02066721859313E-17,2.9));
#8847=CARTESIAN_POINT('Origin',(1.72,0.,3.6));
#8848=CARTESIAN_POINT('Origin',(1.72,0.,2.9));
#8849=CARTESIAN_POINT('Origin',(-3.15958874180017E-16,-1.72,2.9));
#8850=CARTESIAN_POINT('',(-0.165,-1.72,2.9));
#8851=CARTESIAN_POINT('Origin',(-3.15958874180017E-16,-1.72,2.9));
#8852=CARTESIAN_POINT('',(-0.165,-1.72,3.6));
#8853=CARTESIAN_POINT('',(-0.165,-1.72,2.9));
#8854=CARTESIAN_POINT('Origin',(-3.15958874180017E-16,-1.72,3.6));
#8855=CARTESIAN_POINT('Origin',(-3.05311331771918E-16,-1.72,2.9));
#8856=CARTESIAN_POINT('Origin',(0.,0.,2.05));
#8857=CARTESIAN_POINT('',(-1.5,-1.83697019872103E-16,2.05));
#8858=CARTESIAN_POINT('Origin',(0.,0.,2.05));
#8859=CARTESIAN_POINT('',(-1.5,1.83697019872103E-16,3.6));
#8860=CARTESIAN_POINT('',(-1.5,-1.83697019872103E-16,2.05));
#8861=CARTESIAN_POINT('Origin',(0.,0.,3.6));
#8862=CARTESIAN_POINT('Origin',(0.,0.,2.05));
#8863=CARTESIAN_POINT('',(-1.02,-1.2491397351303E-16,2.05));
#8864=CARTESIAN_POINT('Origin',(0.,0.,2.05));
#8865=CARTESIAN_POINT('Origin',(0.,0.,0.9));
#8866=CARTESIAN_POINT('',(-1.02,-1.2491397351303E-16,1.));
#8867=CARTESIAN_POINT('Origin',(0.,0.,1.));
#8868=CARTESIAN_POINT('',(-1.02,-1.2491397351303E-16,0.9));
#8869=CARTESIAN_POINT('Origin',(5.94264068711928,-1.7,2.2));
#8870=CARTESIAN_POINT('',(6.44264068711928,-1.7,2.2));
#8871=CARTESIAN_POINT('',(6.44264068711928,-1.7,3.6));
#8872=CARTESIAN_POINT('',(6.44264068711928,-1.7,2.2));
#8873=CARTESIAN_POINT('',(5.94264068711928,-2.2,3.6));
#8874=CARTESIAN_POINT('Origin',(5.94264068711928,-1.7,3.6));
#8875=CARTESIAN_POINT('',(5.94264068711928,-2.2,2.2));
#8876=CARTESIAN_POINT('',(5.94264068711928,-2.2,2.2));
#8877=CARTESIAN_POINT('Origin',(5.94264068711928,-1.7,2.2));
#8878=CARTESIAN_POINT('Origin',(5.94264068711928,-1.7,2.2));
#8879=CARTESIAN_POINT('',(6.44264068711928,-1.7,2.2));
#8880=CARTESIAN_POINT('Origin',(5.94264068711928,-1.7,2.2));
#8881=CARTESIAN_POINT('',(5.94264068711928,-2.2,2.2));
#8882=CARTESIAN_POINT('Origin',(5.94264068711928,-1.7,3.6));
#8883=CARTESIAN_POINT('Origin',(5.94264068711928,-1.7,2.2));
#8884=CARTESIAN_POINT('',(5.66764068711928,-1.7,2.2));
#8885=CARTESIAN_POINT('Origin',(5.94264068711928,-1.7,2.2));
#8886=CARTESIAN_POINT('Origin',(-1.7,1.7,2.2));
#8887=CARTESIAN_POINT('',(-1.7,2.2,2.2));
#8888=CARTESIAN_POINT('',(-1.7,2.2,3.6));
#8889=CARTESIAN_POINT('',(-1.7,2.2,2.2));
#8890=CARTESIAN_POINT('',(-2.2,1.7,3.6));
#8891=CARTESIAN_POINT('Origin',(-1.7,1.7,3.6));
#8892=CARTESIAN_POINT('',(-2.2,1.7,2.2));
#8893=CARTESIAN_POINT('',(-2.2,1.7,2.2));
#8894=CARTESIAN_POINT('Origin',(-1.7,1.7,2.2));
#8895=CARTESIAN_POINT('Origin',(-1.7,1.7,2.2));
#8896=CARTESIAN_POINT('',(-1.7,2.2,2.2));
#8897=CARTESIAN_POINT('Origin',(-1.7,1.7,2.2));
#8898=CARTESIAN_POINT('',(-2.2,1.7,2.2));
#8899=CARTESIAN_POINT('Origin',(-1.7,1.7,3.6));
#8900=CARTESIAN_POINT('Origin',(-1.7,1.7,2.2));
#8901=CARTESIAN_POINT('',(-1.975,1.7,2.2));
#8902=CARTESIAN_POINT('Origin',(-1.7,1.7,2.2));
#8903=CARTESIAN_POINT('Origin',(-1.7,-1.7,2.2));
#8904=CARTESIAN_POINT('',(-1.7,-2.2,2.2));
#8905=CARTESIAN_POINT('',(-1.7,-2.2,3.6));
#8906=CARTESIAN_POINT('',(-1.7,-2.2,2.2));
#8907=CARTESIAN_POINT('',(-2.2,-1.7,3.6));
#8908=CARTESIAN_POINT('Origin',(-1.7,-1.7,3.6));
#8909=CARTESIAN_POINT('',(-2.2,-1.7,2.2));
#8910=CARTESIAN_POINT('',(-2.2,-1.7,2.2));
#8911=CARTESIAN_POINT('Origin',(-1.7,-1.7,2.2));
#8912=CARTESIAN_POINT('Origin',(-1.7,-1.7,2.2));
#8913=CARTESIAN_POINT('',(-1.7,-2.2,2.2));
#8914=CARTESIAN_POINT('Origin',(-1.7,-1.7,2.2));
#8915=CARTESIAN_POINT('',(-2.2,-1.7,2.2));
#8916=CARTESIAN_POINT('Origin',(-1.7,-1.7,3.6));
#8917=CARTESIAN_POINT('Origin',(-1.7,-1.7,2.2));
#8918=CARTESIAN_POINT('',(-1.975,-1.7,2.2));
#8919=CARTESIAN_POINT('Origin',(-1.7,-1.7,2.2));
#8920=CARTESIAN_POINT('Origin',(5.94264068711928,1.7,2.2));
#8921=CARTESIAN_POINT('',(5.94264068711928,2.2,2.2));
#8922=CARTESIAN_POINT('',(5.94264068711928,2.2,3.6));
#8923=CARTESIAN_POINT('',(5.94264068711928,2.2,2.2));
#8924=CARTESIAN_POINT('',(6.44264068711928,1.7,3.6));
#8925=CARTESIAN_POINT('Origin',(5.94264068711928,1.7,3.6));
#8926=CARTESIAN_POINT('',(6.44264068711928,1.7,2.2));
#8927=CARTESIAN_POINT('',(6.44264068711928,1.7,2.2));
#8928=CARTESIAN_POINT('Origin',(5.94264068711928,1.7,2.2));
#8929=CARTESIAN_POINT('Origin',(5.94264068711928,1.7,2.2));
#8930=CARTESIAN_POINT('',(5.94264068711928,2.2,2.2));
#8931=CARTESIAN_POINT('Origin',(5.94264068711928,1.7,2.2));
#8932=CARTESIAN_POINT('',(6.44264068711928,1.7,2.2));
#8933=CARTESIAN_POINT('Origin',(5.94264068711928,1.7,3.6));
#8934=CARTESIAN_POINT('Origin',(5.94264068711928,1.7,2.2));
#8935=CARTESIAN_POINT('',(5.66764068711928,1.7,2.2));
#8936=CARTESIAN_POINT('Origin',(5.94264068711928,1.7,2.2));
#8937=CARTESIAN_POINT('Origin',(2.12132034355964,0.,3.6));
#8938=CARTESIAN_POINT('',(6.44264068711929,2.2,3.6));
#8939=CARTESIAN_POINT('',(6.44264068711928,-2.2,3.6));
#8940=CARTESIAN_POINT('',(6.44264068711928,2.2,3.6));
#8941=CARTESIAN_POINT('Origin',(2.12132034355964,0.,3.6));
#8942=CARTESIAN_POINT('',(-2.2,-2.2,3.6));
#8943=CARTESIAN_POINT('',(-2.2,2.2,3.6));
#8944=CARTESIAN_POINT('',(-2.2,-2.2,3.6));
#8945=CARTESIAN_POINT('Origin',(2.12132034355964,0.,3.6));
#8946=CARTESIAN_POINT('',(-2.2,2.2,3.6));
#8947=CARTESIAN_POINT('',(6.44264068711928,2.2,3.6));
#8948=CARTESIAN_POINT('',(-2.2,2.2,3.6));
#8949=CARTESIAN_POINT('Origin',(2.12132034355964,0.,3.6));
#8950=CARTESIAN_POINT('',(6.44264068711928,-2.2,3.6));
#8951=CARTESIAN_POINT('',(6.44264068711928,2.2,3.6));
#8952=CARTESIAN_POINT('',(-2.2,2.2,3.6));
#8953=CARTESIAN_POINT('',(-2.2,-2.2,3.6));
#8954=CARTESIAN_POINT('Origin',(2.12132034355964,0.,3.6));
#8955=CARTESIAN_POINT('',(6.44264068711929,-2.2,3.6));
#8956=CARTESIAN_POINT('',(-2.2,-2.2,3.6));
#8957=CARTESIAN_POINT('',(6.44264068711928,-2.2,3.6));
#8958=CARTESIAN_POINT('Origin',(5.94264068711928,-1.7,0.9));
#8959=CARTESIAN_POINT('',(5.66764068711928,-1.7,1.));
#8960=CARTESIAN_POINT('Origin',(5.94264068711928,-1.7,1.));
#8961=CARTESIAN_POINT('',(5.66764068711928,-1.7,0.9));
#8962=CARTESIAN_POINT('Origin',(-1.7,1.7,0.9));
#8963=CARTESIAN_POINT('',(-1.975,1.7,1.));
#8964=CARTESIAN_POINT('Origin',(-1.7,1.7,1.));
#8965=CARTESIAN_POINT('',(-1.975,1.7,0.9));
#8966=CARTESIAN_POINT('Origin',(-1.7,-1.7,0.9));
#8967=CARTESIAN_POINT('',(-1.975,-1.7,1.));
#8968=CARTESIAN_POINT('Origin',(-1.7,-1.7,1.));
#8969=CARTESIAN_POINT('',(-1.975,-1.7,0.9));
#8970=CARTESIAN_POINT('Origin',(5.94264068711928,1.7,0.9));
#8971=CARTESIAN_POINT('',(5.66764068711928,1.7,1.));
#8972=CARTESIAN_POINT('Origin',(5.94264068711928,1.7,1.));
#8973=CARTESIAN_POINT('',(5.66764068711928,1.7,0.9));
#8974=CARTESIAN_POINT('Origin',(6.44264068711928,2.2,1.));
#8975=CARTESIAN_POINT('',(6.44264068711928,2.2,1.));
#8976=CARTESIAN_POINT('',(-2.2,2.2,1.));
#8977=CARTESIAN_POINT('',(6.44264068711928,2.2,1.));
#8978=CARTESIAN_POINT('',(-2.2,2.2,1.));
#8979=CARTESIAN_POINT('',(6.44264068711928,2.2,1.));
#8980=CARTESIAN_POINT('Origin',(6.44264068711928,-2.2,1.));
#8981=CARTESIAN_POINT('',(6.44264068711928,-2.2,1.));
#8982=CARTESIAN_POINT('',(6.44264068711928,-2.2,1.));
#8983=CARTESIAN_POINT('',(6.44264068711928,-2.2,1.));
#8984=CARTESIAN_POINT('Origin',(-2.2,-2.2,1.));
#8985=CARTESIAN_POINT('',(-2.2,-2.2,1.));
#8986=CARTESIAN_POINT('',(-2.2,-2.2,1.));
#8987=CARTESIAN_POINT('',(-2.2,-2.2,1.));
#8988=CARTESIAN_POINT('Origin',(-2.2,2.2,1.));
#8989=CARTESIAN_POINT('',(-2.2,2.2,1.));
#8990=CARTESIAN_POINT('Origin',(2.12132034355964,0.,1.));
#8991=CARTESIAN_POINT('',(0.,0.,0.));
#8992=CARTESIAN_POINT('Origin',(-1.72,2.10639249453345E-16,4.));
#8993=CARTESIAN_POINT('',(-1.9819113372093,0.268379305165721,4.));
#8994=CARTESIAN_POINT('',(-1.9819113372093,0.26837930516572,4.4));
#8995=CARTESIAN_POINT('',(-1.9819113372093,0.268379305165721,4.));
#8996=CARTESIAN_POINT('',(-1.9819113372093,-0.268379305165721,4.));
#8997=CARTESIAN_POINT('Origin',(-1.72,2.10639249453345E-16,4.));
#8998=CARTESIAN_POINT('',(-1.9819113372093,-0.268379305165719,4.4));
#8999=CARTESIAN_POINT('',(-1.9819113372093,-0.268379305165721,4.));
#9000=CARTESIAN_POINT('Origin',(-1.72,2.10639249453345E-16,4.4));
#9001=CARTESIAN_POINT('Origin',(-1.72,2.22044604925031E-16,4.));
#9002=CARTESIAN_POINT('',(-2.,-2.44929359829471E-16,4.));
#9003=CARTESIAN_POINT('Origin',(0.,0.,4.));
#9004=CARTESIAN_POINT('Origin',(0.,0.,4.));
#9005=CARTESIAN_POINT('',(-1.945,1.83084696472529E-16,4.));
#9006=CARTESIAN_POINT('Origin',(-1.72,2.10639249453345E-16,4.));
#9007=CARTESIAN_POINT('Origin',(1.11022302462516E-16,1.72,4.));
#9008=CARTESIAN_POINT('',(-0.268379305165721,1.9819113372093,4.));
#9009=CARTESIAN_POINT('',(0.268379305165721,1.9819113372093,4.));
#9010=CARTESIAN_POINT('Origin',(0.,0.,4.));
#9011=CARTESIAN_POINT('Origin',(1.05319624726672E-16,1.72,4.));
#9012=CARTESIAN_POINT('',(-0.225,1.72,4.));
#9013=CARTESIAN_POINT('Origin',(1.05319624726672E-16,1.72,4.));
#9014=CARTESIAN_POINT('Origin',(1.05319624726672E-16,1.72,4.));
#9015=CARTESIAN_POINT('',(-0.26837930516572,1.9819113372093,4.4));
#9016=CARTESIAN_POINT('',(-0.268379305165721,1.9819113372093,4.));
#9017=CARTESIAN_POINT('',(0.26837930516572,1.9819113372093,4.4));
#9018=CARTESIAN_POINT('Origin',(1.05319624726672E-16,1.72,4.4));
#9019=CARTESIAN_POINT('',(0.268379305165721,1.9819113372093,4.));
#9020=CARTESIAN_POINT('Origin',(1.72,0.,4.));
#9021=CARTESIAN_POINT('',(1.9819113372093,0.268379305165721,4.));
#9022=CARTESIAN_POINT('',(1.9819113372093,-0.268379305165721,4.));
#9023=CARTESIAN_POINT('Origin',(0.,0.,4.));
#9024=CARTESIAN_POINT('Origin',(1.72,0.,4.));
#9025=CARTESIAN_POINT('',(1.495,-2.75545529808155E-17,4.));
#9026=CARTESIAN_POINT('Origin',(1.72,0.,4.));
#9027=CARTESIAN_POINT('Origin',(1.72,0.,4.));
#9028=CARTESIAN_POINT('',(1.9819113372093,0.26837930516572,4.4));
#9029=CARTESIAN_POINT('',(1.9819113372093,0.268379305165721,4.));
#9030=CARTESIAN_POINT('',(1.9819113372093,-0.26837930516572,4.4));
#9031=CARTESIAN_POINT('Origin',(1.72,0.,4.4));
#9032=CARTESIAN_POINT('',(1.9819113372093,-0.268379305165721,4.));
#9033=CARTESIAN_POINT('Origin',(-3.33066907387547E-16,-1.72,4.));
#9034=CARTESIAN_POINT('',(0.26837930516572,-1.9819113372093,4.));
#9035=CARTESIAN_POINT('',(-0.268379305165721,-1.9819113372093,4.));
#9036=CARTESIAN_POINT('Origin',(0.,0.,4.));
#9037=CARTESIAN_POINT('Origin',(-3.15958874180017E-16,-1.72,4.));
#9038=CARTESIAN_POINT('',(-0.225,-1.72,4.));
#9039=CARTESIAN_POINT('Origin',(-3.15958874180017E-16,-1.72,4.));
#9040=CARTESIAN_POINT('Origin',(-3.15958874180017E-16,-1.72,4.));
#9041=CARTESIAN_POINT('',(0.268379305165719,-1.9819113372093,4.4));
#9042=CARTESIAN_POINT('',(0.26837930516572,-1.9819113372093,4.));
#9043=CARTESIAN_POINT('',(-0.26837930516572,-1.9819113372093,4.4));
#9044=CARTESIAN_POINT('Origin',(-3.15958874180017E-16,-1.72,4.4));
#9045=CARTESIAN_POINT('',(-0.268379305165721,-1.9819113372093,4.));
#9046=CARTESIAN_POINT('Origin',(0.,0.,4.4));
#9047=CARTESIAN_POINT('Origin',(0.,0.,4.4));
#9048=CARTESIAN_POINT('Origin',(0.,0.,4.4));
#9049=CARTESIAN_POINT('Origin',(0.,0.,4.4));
#9050=CARTESIAN_POINT('Origin',(0.,0.,4.4));
#9051=CARTESIAN_POINT('',(-0.71,-8.69499227394621E-17,4.4));
#9052=CARTESIAN_POINT('Origin',(0.,0.,4.4));
#9053=CARTESIAN_POINT('Origin',(-1.72,2.10639249453345E-16,3.5));
#9054=CARTESIAN_POINT('',(-1.945,1.83084696472529E-16,3.6));
#9055=CARTESIAN_POINT('Origin',(-1.72,2.10639249453345E-16,3.6));
#9056=CARTESIAN_POINT('',(-1.945,1.83084696472529E-16,3.5));
#9057=CARTESIAN_POINT('Origin',(1.05319624726672E-16,1.72,3.5));
#9058=CARTESIAN_POINT('',(-0.225,1.72,3.6));
#9059=CARTESIAN_POINT('Origin',(1.05319624726672E-16,1.72,3.6));
#9060=CARTESIAN_POINT('',(-0.225,1.72,3.5));
#9061=CARTESIAN_POINT('Origin',(1.72,0.,3.5));
#9062=CARTESIAN_POINT('',(1.495,-2.75545529808155E-17,3.6));
#9063=CARTESIAN_POINT('Origin',(1.72,0.,3.6));
#9064=CARTESIAN_POINT('',(1.495,-2.75545529808155E-17,3.5));
#9065=CARTESIAN_POINT('Origin',(-3.15958874180017E-16,-1.72,3.5));
#9066=CARTESIAN_POINT('',(-0.225,-1.72,3.6));
#9067=CARTESIAN_POINT('Origin',(-3.15958874180017E-16,-1.72,3.6));
#9068=CARTESIAN_POINT('',(-0.225,-1.72,3.5));
#9069=CARTESIAN_POINT('Origin',(0.,0.,2.95));
#9070=CARTESIAN_POINT('',(-1.49,-1.82472373072956E-16,3.6));
#9071=CARTESIAN_POINT('Origin',(0.,0.,3.6));
#9072=CARTESIAN_POINT('',(-1.49,-1.82472373072956E-16,2.95));
#9073=CARTESIAN_POINT('',(-1.49,-1.82472373072956E-16,2.95));
#9074=CARTESIAN_POINT('Origin',(0.,0.,2.95));
#9075=CARTESIAN_POINT('Origin',(0.,0.,2.95));
#9076=CARTESIAN_POINT('',(-0.71,-8.69499227394621E-17,2.95));
#9077=CARTESIAN_POINT('Origin',(0.,0.,2.95));
#9078=CARTESIAN_POINT('Origin',(0.,0.,3.6));
#9079=CARTESIAN_POINT('',(-0.71,-8.69499227394621E-17,3.6));
#9080=CARTESIAN_POINT('Origin',(0.,0.,3.6));
#9081=CARTESIAN_POINT('',(-2.,-2.44929359829471E-16,3.6));
#9082=CARTESIAN_POINT('',(-2.,-2.44929359829471E-16,3.6));
#9083=CARTESIAN_POINT('Origin',(0.,0.,3.6));
#9084=CARTESIAN_POINT('Origin',(0.,0.,3.6));
#9085=CARTESIAN_POINT('',(0.,0.,0.));
#9086=CARTESIAN_POINT('Origin',(2.52264068711929,2.10639249453345E-16,4.));
#9087=CARTESIAN_POINT('',(2.26072934990998,0.268379305165721,4.));
#9088=CARTESIAN_POINT('',(2.26072934990998,0.268379305165722,4.4));
#9089=CARTESIAN_POINT('',(2.26072934990998,0.268379305165721,4.));
#9090=CARTESIAN_POINT('',(2.26072934990998,-0.268379305165721,4.));
#9091=CARTESIAN_POINT('Origin',(2.52264068711929,2.10639249453345E-16,4.));
#9092=CARTESIAN_POINT('',(2.26072934990998,-0.268379305165721,4.4));
#9093=CARTESIAN_POINT('',(2.26072934990998,-0.268379305165721,4.));
#9094=CARTESIAN_POINT('Origin',(2.52264068711929,2.10639249453345E-16,4.4));
#9095=CARTESIAN_POINT('Origin',(2.52264068711929,2.22044604925031E-16,4.));
#9096=CARTESIAN_POINT('',(2.24264068711929,-2.44929359829471E-16,4.));
#9097=CARTESIAN_POINT('Origin',(4.24264068711929,0.,4.));
#9098=CARTESIAN_POINT('Origin',(4.24264068711929,0.,4.));
#9099=CARTESIAN_POINT('',(2.29764068711929,1.83084696472529E-16,4.));
#9100=CARTESIAN_POINT('Origin',(2.52264068711929,2.10639249453345E-16,4.));
#9101=CARTESIAN_POINT('Origin',(4.24264068711929,1.72,4.));
#9102=CARTESIAN_POINT('',(3.97426138195357,1.9819113372093,4.));
#9103=CARTESIAN_POINT('',(4.51101999228501,1.9819113372093,4.));
#9104=CARTESIAN_POINT('Origin',(4.24264068711929,0.,4.));
#9105=CARTESIAN_POINT('Origin',(4.24264068711929,1.72,4.));
#9106=CARTESIAN_POINT('',(4.01764068711929,1.72,4.));
#9107=CARTESIAN_POINT('Origin',(4.24264068711929,1.72,4.));
#9108=CARTESIAN_POINT('Origin',(4.24264068711929,1.72,4.));
#9109=CARTESIAN_POINT('',(3.97426138195357,1.9819113372093,4.4));
#9110=CARTESIAN_POINT('',(3.97426138195357,1.9819113372093,4.));
#9111=CARTESIAN_POINT('',(4.51101999228501,1.9819113372093,4.4));
#9112=CARTESIAN_POINT('Origin',(4.24264068711929,1.72,4.4));
#9113=CARTESIAN_POINT('',(4.51101999228501,1.9819113372093,4.));
#9114=CARTESIAN_POINT('Origin',(5.96264068711929,0.,4.));
#9115=CARTESIAN_POINT('',(6.22455202432859,0.268379305165721,4.));
#9116=CARTESIAN_POINT('',(6.22455202432859,-0.268379305165721,4.));
#9117=CARTESIAN_POINT('Origin',(4.24264068711929,0.,4.));
#9118=CARTESIAN_POINT('Origin',(5.96264068711929,0.,4.));
#9119=CARTESIAN_POINT('',(5.73764068711929,-2.75545529808154E-17,4.));
#9120=CARTESIAN_POINT('Origin',(5.96264068711929,0.,4.));
#9121=CARTESIAN_POINT('Origin',(5.96264068711929,0.,4.));
#9122=CARTESIAN_POINT('',(6.22455202432859,0.26837930516572,4.4));
#9123=CARTESIAN_POINT('',(6.22455202432859,0.268379305165721,4.));
#9124=CARTESIAN_POINT('',(6.22455202432859,-0.26837930516572,4.4));
#9125=CARTESIAN_POINT('Origin',(5.96264068711929,0.,4.4));
#9126=CARTESIAN_POINT('',(6.22455202432859,-0.268379305165721,4.));
#9127=CARTESIAN_POINT('Origin',(4.24264068711929,-1.72,4.));
#9128=CARTESIAN_POINT('',(4.51101999228501,-1.9819113372093,4.));
#9129=CARTESIAN_POINT('',(3.97426138195357,-1.9819113372093,4.));
#9130=CARTESIAN_POINT('Origin',(4.24264068711929,0.,4.));
#9131=CARTESIAN_POINT('Origin',(4.24264068711929,-1.72,4.));
#9132=CARTESIAN_POINT('',(4.01764068711929,-1.72,4.));
#9133=CARTESIAN_POINT('Origin',(4.24264068711929,-1.72,4.));
#9134=CARTESIAN_POINT('Origin',(4.24264068711929,-1.72,4.));
#9135=CARTESIAN_POINT('',(4.51101999228501,-1.9819113372093,4.4));
#9136=CARTESIAN_POINT('',(4.51101999228501,-1.9819113372093,4.));
#9137=CARTESIAN_POINT('',(3.97426138195357,-1.9819113372093,4.4));
#9138=CARTESIAN_POINT('Origin',(4.24264068711929,-1.72,4.4));
#9139=CARTESIAN_POINT('',(3.97426138195357,-1.9819113372093,4.));
#9140=CARTESIAN_POINT('Origin',(4.24264068711929,0.,4.4));
#9141=CARTESIAN_POINT('Origin',(4.24264068711929,0.,4.4));
#9142=CARTESIAN_POINT('Origin',(4.24264068711929,0.,4.4));
#9143=CARTESIAN_POINT('Origin',(4.24264068711929,0.,4.4));
#9144=CARTESIAN_POINT('Origin',(4.24264068711929,0.,4.4));
#9145=CARTESIAN_POINT('',(3.53264068711929,-8.69499227394621E-17,4.4));
#9146=CARTESIAN_POINT('Origin',(4.24264068711929,0.,4.4));
#9147=CARTESIAN_POINT('Origin',(2.52264068711929,2.10639249453345E-16,3.5));
#9148=CARTESIAN_POINT('',(2.29764068711929,1.83084696472529E-16,3.6));
#9149=CARTESIAN_POINT('Origin',(2.52264068711929,2.10639249453345E-16,3.6));
#9150=CARTESIAN_POINT('',(2.29764068711929,1.83084696472529E-16,3.5));
#9151=CARTESIAN_POINT('Origin',(4.24264068711929,1.72,3.5));
#9152=CARTESIAN_POINT('',(4.01764068711929,1.72,3.6));
#9153=CARTESIAN_POINT('Origin',(4.24264068711929,1.72,3.6));
#9154=CARTESIAN_POINT('',(4.01764068711929,1.72,3.5));
#9155=CARTESIAN_POINT('Origin',(5.96264068711929,0.,3.5));
#9156=CARTESIAN_POINT('',(5.73764068711929,-2.75545529808154E-17,3.6));
#9157=CARTESIAN_POINT('Origin',(5.96264068711929,0.,3.6));
#9158=CARTESIAN_POINT('',(5.73764068711929,-2.75545529808154E-17,3.5));
#9159=CARTESIAN_POINT('Origin',(4.24264068711929,-1.72,3.5));
#9160=CARTESIAN_POINT('',(4.01764068711929,-1.72,3.6));
#9161=CARTESIAN_POINT('Origin',(4.24264068711929,-1.72,3.6));
#9162=CARTESIAN_POINT('',(4.01764068711929,-1.72,3.5));
#9163=CARTESIAN_POINT('Origin',(4.24264068711929,0.,2.95));
#9164=CARTESIAN_POINT('',(2.75264068711929,-1.82472373072956E-16,3.6));
#9165=CARTESIAN_POINT('Origin',(4.24264068711929,0.,3.6));
#9166=CARTESIAN_POINT('',(2.75264068711929,-1.82472373072956E-16,2.95));
#9167=CARTESIAN_POINT('',(2.75264068711929,-1.82472373072956E-16,2.95));
#9168=CARTESIAN_POINT('Origin',(4.24264068711929,0.,2.95));
#9169=CARTESIAN_POINT('Origin',(4.24264068711929,0.,2.95));
#9170=CARTESIAN_POINT('',(3.53264068711929,-8.69499227394621E-17,2.95));
#9171=CARTESIAN_POINT('Origin',(4.24264068711929,0.,2.95));
#9172=CARTESIAN_POINT('Origin',(4.24264068711929,0.,3.6));
#9173=CARTESIAN_POINT('',(3.53264068711929,-8.69499227394621E-17,3.6));
#9174=CARTESIAN_POINT('Origin',(4.24264068711929,0.,3.6));
#9175=CARTESIAN_POINT('',(2.24264068711929,-2.44929359829471E-16,3.6));
#9176=CARTESIAN_POINT('',(2.24264068711929,-2.44929359829471E-16,3.6));
#9177=CARTESIAN_POINT('Origin',(4.24264068711929,0.,3.6));
#9178=CARTESIAN_POINT('Origin',(4.24264068711929,0.,3.6));
#9179=CARTESIAN_POINT('',(0.,0.,0.));
#9180=CARTESIAN_POINT('Origin',(0.375,0.5,0.));
#9181=CARTESIAN_POINT('',(-0.375,0.5,-4.59242549680257E-17));
#9182=CARTESIAN_POINT('Origin',(0.,0.5,0.));
#9183=CARTESIAN_POINT('Origin',(0.,0.475,0.));
#9184=CARTESIAN_POINT('',(-0.425,0.45,-5.20474889637625E-17));
#9185=CARTESIAN_POINT('Origin',(0.,0.45,0.));
#9186=CARTESIAN_POINT('',(-0.4,0.475,-4.89858719658941E-17));
#9187=CARTESIAN_POINT('Origin',(0.,0.24,0.));
#9188=CARTESIAN_POINT('',(-0.425,0.0299999999999998,-5.20474889637625E-17));
#9189=CARTESIAN_POINT('Origin',(0.,0.0299999999999998,0.));
#9190=CARTESIAN_POINT('',(-0.425,0.24,-5.20474889637625E-17));
#9191=CARTESIAN_POINT('Origin',(0.,0.0150000000000001,0.));
#9192=CARTESIAN_POINT('',(-0.395,4.85722573273506E-17,-4.83735485663204E-17));
#9193=CARTESIAN_POINT('Origin',(0.,0.,0.));
#9194=CARTESIAN_POINT('',(-0.41,0.0150000000000001,-5.02105187650415E-17));
#9195=CARTESIAN_POINT('Origin',(0.27,0.,0.));
#9196=CARTESIAN_POINT('',(-0.27,0.,-3.30654635769785E-17));
#9197=CARTESIAN_POINT('Origin',(0.,0.,0.));
#9198=CARTESIAN_POINT('Origin',(0.,-0.02,0.));
#9199=CARTESIAN_POINT('',(-0.24505,-0.0498999999999999,3.00099698131059E-17));
#9200=CARTESIAN_POINT('Origin',(0.,-0.0498999999999999,0.));
#9201=CARTESIAN_POINT('',(-0.26,-0.02,-3.18408167778312E-17));
#9202=CARTESIAN_POINT('Origin',(0.,-0.995,0.));
#9203=CARTESIAN_POINT('',(-0.24505,-1.95495,3.00099698131059E-17));
#9204=CARTESIAN_POINT('Origin',(0.,-1.95495,0.));
#9205=CARTESIAN_POINT('',(-0.24505,-0.995,-3.00099698131059E-17));
#9206=CARTESIAN_POINT('Origin',(0.,-1.975,0.));
#9207=CARTESIAN_POINT('',(-0.2,-2.,-2.44929359829471E-17));
#9208=CARTESIAN_POINT('Origin',(0.,-2.,0.));
#9209=CARTESIAN_POINT('',(-0.225,-1.975,-2.75545529808154E-17));
#9210=CARTESIAN_POINT('Origin',(0.,-2.,0.));
#9211=CARTESIAN_POINT('Origin',(0.115470053837925,-0.5,-0.2));
#9212=CARTESIAN_POINT('',(0.23094010767585,-0.5,0.));
#9213=CARTESIAN_POINT('',(0.115470053837925,-0.5,-0.2));
#9214=CARTESIAN_POINT('',(0.23094010767585,-0.5,0.));
#9215=CARTESIAN_POINT('',(0.115470053837925,-0.8,-0.2));
#9216=CARTESIAN_POINT('',(0.115470053837925,-0.5,-0.2));
#9217=CARTESIAN_POINT('',(0.23094010767585,-0.8,0.));
#9218=CARTESIAN_POINT('',(0.23094010767585,-0.8,0.));
#9219=CARTESIAN_POINT('',(0.23094010767585,-0.5,0.));
#9220=CARTESIAN_POINT('Origin',(-0.115470053837925,-0.5,-0.2));
#9221=CARTESIAN_POINT('',(-0.115470053837925,-0.5,-0.2));
#9222=CARTESIAN_POINT('',(0.115470053837925,-0.5,-0.2));
#9223=CARTESIAN_POINT('',(-0.115470053837925,-0.8,-0.2));
#9224=CARTESIAN_POINT('',(-0.115470053837925,-0.5,-0.2));
#9225=CARTESIAN_POINT('',(0.115470053837925,-0.8,-0.2));
#9226=CARTESIAN_POINT('Origin',(-0.23094010767585,-0.5,-2.77555756156289E-17));
#9227=CARTESIAN_POINT('',(-0.23094010767585,-0.5,-2.82820063659975E-17));
#9228=CARTESIAN_POINT('',(-0.115470053837925,-0.5,-0.2));
#9229=CARTESIAN_POINT('',(-0.23094010767585,-0.8,-2.77555756156289E-17));
#9230=CARTESIAN_POINT('',(-0.23094010767585,-0.5,-2.82820063659975E-17));
#9231=CARTESIAN_POINT('',(-0.115470053837925,-0.8,-0.2));
#9232=CARTESIAN_POINT('Origin',(-0.115470053837925,-0.5,0.2));
#9233=CARTESIAN_POINT('',(-0.115470053837925,-0.5,0.2));
#9234=CARTESIAN_POINT('',(-0.23094010767585,-0.5,-2.82820063659975E-17));
#9235=CARTESIAN_POINT('',(-0.115470053837925,-0.8,0.2));
#9236=CARTESIAN_POINT('',(-0.115470053837925,-0.5,0.2));
#9237=CARTESIAN_POINT('',(-0.23094010767585,-0.8,-2.82820063659975E-17));
#9238=CARTESIAN_POINT('Origin',(0.115470053837925,-0.5,0.2));
#9239=CARTESIAN_POINT('',(0.115470053837925,-0.5,0.2));
#9240=CARTESIAN_POINT('',(-0.115470053837925,-0.5,0.2));
#9241=CARTESIAN_POINT('',(0.115470053837925,-0.8,0.2));
#9242=CARTESIAN_POINT('',(0.115470053837925,-0.5,0.2));
#9243=CARTESIAN_POINT('',(-0.115470053837925,-0.8,0.2));
#9244=CARTESIAN_POINT('Origin',(0.23094010767585,-0.5,0.));
#9245=CARTESIAN_POINT('',(0.115470053837925,-0.5,0.2));
#9246=CARTESIAN_POINT('',(0.115470053837925,-0.8,0.2));
#9247=CARTESIAN_POINT('Origin',(0.,-0.5,0.));
#9248=CARTESIAN_POINT('Origin',(0.,-0.8,0.));
#9249=CARTESIAN_POINT('',(0.,0.,0.));
#9250=CARTESIAN_POINT('',(0.,0.,0.));
#9251=CARTESIAN_POINT('Origin',(0.,0.,0.));
#9252=CARTESIAN_POINT('',(-0.976185,-0.246528389340863,-1.19548183562566E-16));
#9253=CARTESIAN_POINT('',(-1.19548183562566E-16,-0.246528389340863,0.976185));
#9254=CARTESIAN_POINT('Origin',(0.,-0.246528389340863,0.));
#9255=CARTESIAN_POINT('Origin',(0.,-0.246528389340863,0.));
#9256=CARTESIAN_POINT('',(-1.19548183562566E-16,0.246528389340863,0.976185));
#9257=CARTESIAN_POINT('Origin',(-1.22464679914735E-16,0.,1.));
#9258=CARTESIAN_POINT('',(-0.976185,0.246528389340863,1.19548183562566E-16));
#9259=CARTESIAN_POINT('Origin',(0.,0.246528389340863,0.));
#9260=CARTESIAN_POINT('Origin',(0.,0.246528389340863,0.));
#9261=CARTESIAN_POINT('Origin',(0.,0.,0.));
#9262=CARTESIAN_POINT('',(-0.976185,0.45,-1.19548183562566E-16));
#9263=CARTESIAN_POINT('',(-0.976185,0.,-1.19548183562566E-16));
#9264=CARTESIAN_POINT('Origin',(0.,0.45,0.));
#9265=CARTESIAN_POINT('Origin',(0.,0.,0.));
#9266=CARTESIAN_POINT('',(-0.5,-0.39,-6.12323399573677E-17));
#9267=CARTESIAN_POINT('Origin',(0.,-0.39,0.));
#9268=CARTESIAN_POINT('',(-0.5,0.39,-6.12323399573677E-17));
#9269=CARTESIAN_POINT('',(-0.5,0.,-6.12323399573677E-17));
#9270=CARTESIAN_POINT('Origin',(0.,0.39,0.));
#9271=CARTESIAN_POINT('Origin',(0.,0.42,0.));
#9272=CARTESIAN_POINT('',(-0.56,0.45,-6.85802207522518E-17));
#9273=CARTESIAN_POINT('',(-0.53,0.42,-6.49062803548097E-17));
#9274=CARTESIAN_POINT('Origin',(0.,0.45,0.));
#9275=CARTESIAN_POINT('Origin',(0.976185,0.45,0.));
#9276=CARTESIAN_POINT('Origin',(0.,0.,0.));
#9277=CARTESIAN_POINT('',(-0.976185,-0.45,-1.19548183562566E-16));
#9278=CARTESIAN_POINT('Origin',(0.,-0.45,0.));
#9279=CARTESIAN_POINT('',(-0.976185,0.,-1.19548183562566E-16));
#9280=CARTESIAN_POINT('Origin',(0.56,-0.45,0.));
#9281=CARTESIAN_POINT('',(-0.56,-0.45,-6.85802207522518E-17));
#9282=CARTESIAN_POINT('Origin',(0.,-0.45,0.));
#9283=CARTESIAN_POINT('Origin',(0.,-0.42,0.));
#9284=CARTESIAN_POINT('',(-0.53,-0.42,-6.49062803548097E-17));
#9285=CARTESIAN_POINT('',(0.,0.,0.));
#9286=CARTESIAN_POINT('Origin',(0.,0.,0.));
#9287=CARTESIAN_POINT('',(-1.023815,0.246528389340863,-1.25381176266905E-16));
#9288=CARTESIAN_POINT('',(-1.25381176266905E-16,0.246528389340863,1.023815));
#9289=CARTESIAN_POINT('Origin',(0.,0.246528389340863,0.));
#9290=CARTESIAN_POINT('Origin',(0.,0.246528389340863,0.));
#9291=CARTESIAN_POINT('',(-1.25381176266905E-16,-0.246528389340863,1.023815));
#9292=CARTESIAN_POINT('Origin',(-1.22464679914735E-16,0.,1.));
#9293=CARTESIAN_POINT('',(-1.023815,-0.246528389340863,1.25381176266905E-16));
#9294=CARTESIAN_POINT('Origin',(0.,-0.246528389340863,0.));
#9295=CARTESIAN_POINT('Origin',(0.,-0.246528389340863,0.));
#9296=CARTESIAN_POINT('Origin',(0.,0.,0.));
#9297=CARTESIAN_POINT('',(-1.023815,-0.45,-1.25381176266905E-16));
#9298=CARTESIAN_POINT('Origin',(0.,-0.45,0.));
#9299=CARTESIAN_POINT('',(-1.023815,0.,-1.25381176266905E-16));
#9300=CARTESIAN_POINT('Origin',(1.44,0.45,0.));
#9301=CARTESIAN_POINT('',(-1.44,0.45,-1.76349139077219E-16));
#9302=CARTESIAN_POINT('Origin',(0.,0.45,0.));
#9303=CARTESIAN_POINT('',(-1.023815,0.45,-1.25381176266905E-16));
#9304=CARTESIAN_POINT('Origin',(0.,0.45,0.));
#9305=CARTESIAN_POINT('Origin',(0.,0.42,0.));
#9306=CARTESIAN_POINT('',(-1.5,0.39,-1.83697019872103E-16));
#9307=CARTESIAN_POINT('Origin',(0.,0.39,0.));
#9308=CARTESIAN_POINT('',(-1.47,0.42,-1.80023079474661E-16));
#9309=CARTESIAN_POINT('Origin',(0.,0.,0.));
#9310=CARTESIAN_POINT('',(-1.5,-0.39,-1.83697019872103E-16));
#9311=CARTESIAN_POINT('Origin',(0.,-0.39,0.));
#9312=CARTESIAN_POINT('',(-1.5,0.,-1.83697019872103E-16));
#9313=CARTESIAN_POINT('Origin',(0.,-0.42,0.));
#9314=CARTESIAN_POINT('',(-1.44,-0.45,-1.76349139077219E-16));
#9315=CARTESIAN_POINT('Origin',(0.,-0.45,0.));
#9316=CARTESIAN_POINT('',(-1.47,-0.42,-1.80023079474661E-16));
#9317=CARTESIAN_POINT('Origin',(1.023815,-0.45,0.));
#9318=CARTESIAN_POINT('Origin',(0.,0.,0.));
#9319=CARTESIAN_POINT('',(-1.023815,0.,-1.25381176266905E-16));
#9320=CARTESIAN_POINT('',(0.,0.,0.));
#9321=CARTESIAN_POINT('Origin',(1.,0.,0.));
#9322=CARTESIAN_POINT('',(1.,-1.78583896120461E-33,0.23815));
#9323=CARTESIAN_POINT('',(1.,-1.78583896120461E-33,-0.23815));
#9324=CARTESIAN_POINT('Origin',(1.,0.,0.));
#9325=CARTESIAN_POINT('Origin',(0.707106781186548,0.,-0.707106781186547));
#9326=CARTESIAN_POINT('',(0.875504261126124,-1.78583896120461E-33,-0.538709301246971));
#9327=CARTESIAN_POINT('',(0.538709301246971,-1.78583896120461E-33,-0.875504261126124));
#9328=CARTESIAN_POINT('Origin',(0.707106781186548,0.,-0.707106781186547));
#9329=CARTESIAN_POINT('Origin',(6.12323399573677E-17,0.,-1.));
#9330=CARTESIAN_POINT('',(0.23815,-1.78583896120461E-33,-1.));
#9331=CARTESIAN_POINT('',(-0.23815,-1.78583896120461E-33,-1.));
#9332=CARTESIAN_POINT('Origin',(6.12323399573677E-17,0.,-1.));
#9333=CARTESIAN_POINT('Origin',(-0.707106781186547,0.,-0.707106781186548));
#9334=CARTESIAN_POINT('',(-0.538709301246971,-1.78583896120461E-33,-0.875504261126124));
#9335=CARTESIAN_POINT('',(-0.875504261126124,-1.78583896120461E-33,-0.538709301246971));
#9336=CARTESIAN_POINT('Origin',(-0.707106781186547,0.,-0.707106781186548));
#9337=CARTESIAN_POINT('Origin',(-1.,0.,-1.22464679914735E-16));
#9338=CARTESIAN_POINT('',(-1.,-1.78583896120461E-33,-0.23815));
#9339=CARTESIAN_POINT('',(-1.,-1.78583896120461E-33,0.23815));
#9340=CARTESIAN_POINT('Origin',(-1.,0.,-1.22464679914735E-16));
#9341=CARTESIAN_POINT('Origin',(-0.707106781186548,0.,0.707106781186547));
#9342=CARTESIAN_POINT('',(-0.875504261126124,-7.94881478324376E-33,0.538709301246971));
#9343=CARTESIAN_POINT('',(-0.538709301246971,4.37713686083455E-33,0.875504261126124));
#9344=CARTESIAN_POINT('Origin',(-0.707106781186548,0.,0.707106781186547));
#9345=CARTESIAN_POINT('Origin',(-1.83697019872103E-16,0.,1.));
#9346=CARTESIAN_POINT('',(-0.23815,-1.78583896120461E-33,1.));
#9347=CARTESIAN_POINT('',(0.23815,-1.78583896120461E-33,1.));
#9348=CARTESIAN_POINT('Origin',(-1.83697019872103E-16,0.,1.));
#9349=CARTESIAN_POINT('Origin',(0.707106781186547,0.,0.707106781186548));
#9350=CARTESIAN_POINT('',(0.538709301246971,-4.86732687222419E-33,0.875504261126124));
#9351=CARTESIAN_POINT('',(0.875504261126124,1.29564894981497E-33,0.538709301246971));
#9352=CARTESIAN_POINT('Origin',(0.707106781186547,0.,0.707106781186548));
#9353=CARTESIAN_POINT('',(0.,0.,0.));
#9354=CARTESIAN_POINT('Origin',(0.707106781186547,0.,0.707106781186548));
#9355=CARTESIAN_POINT('',(0.504455939115715,-0.04763,0.841298510752802));
#9356=CARTESIAN_POINT('',(0.841298510752802,-0.04763,0.504455939115715));
#9357=CARTESIAN_POINT('Ctrl Pts',(0.504455939115715,-0.04763,0.841298510752802));
#9358=CARTESIAN_POINT('Ctrl Pts',(0.508899795931835,-0.0740444353928835,
0.838633903678357));
#9359=CARTESIAN_POINT('Ctrl Pts',(0.517157748491652,-0.0999305678883309,
0.833661031856294));
#9360=CARTESIAN_POINT('Ctrl Pts',(0.537715343527944,-0.142345102874864,
0.820511285096538));
#9361=CARTESIAN_POINT('Ctrl Pts',(0.548874290046456,-0.159766064500479,
0.813159949759));
#9362=CARTESIAN_POINT('Ctrl Pts',(0.573915184558107,-0.190326085855194,
0.795684265985089));
#9363=CARTESIAN_POINT('Ctrl Pts',(0.587792702767295,-0.203463743702801,
0.78555112003688));
#9364=CARTESIAN_POINT('Ctrl Pts',(0.615966552324775,-0.224161999508995,
0.763642258217233));
#9365=CARTESIAN_POINT('Ctrl Pts',(0.631684198665438,-0.232861760990032,
0.750785745543687));
#9366=CARTESIAN_POINT('Ctrl Pts',(0.663382628119203,-0.244251601209411,
0.722929908501543));
#9367=CARTESIAN_POINT('Ctrl Pts',(0.679352081686668,-0.246942143572133,
0.707917883896095));
#9368=CARTESIAN_POINT('Ctrl Pts',(0.707917883896095,-0.246942143572133,
0.679352081686668));
#9369=CARTESIAN_POINT('Ctrl Pts',(0.722929908501543,-0.244251601209411,
0.663382628119203));
#9370=CARTESIAN_POINT('Ctrl Pts',(0.750785745543687,-0.232861760990032,
0.631684198665439));
#9371=CARTESIAN_POINT('Ctrl Pts',(0.763642258217232,-0.224161999508995,
0.615966552324775));
#9372=CARTESIAN_POINT('Ctrl Pts',(0.78555112003688,-0.203463743702801,0.587792702767295));
#9373=CARTESIAN_POINT('Ctrl Pts',(0.795684265985088,-0.190326085855194,
0.573915184558108));
#9374=CARTESIAN_POINT('Ctrl Pts',(0.813159949759,-0.15976606450048,0.548874290046456));
#9375=CARTESIAN_POINT('Ctrl Pts',(0.820511285096538,-0.142345102874864,
0.537715343527944));
#9376=CARTESIAN_POINT('Ctrl Pts',(0.833661031856294,-0.099930567888331,
0.517157748491653));
#9377=CARTESIAN_POINT('Ctrl Pts',(0.838633903678357,-0.0740444353928835,
0.508899795931835));
#9378=CARTESIAN_POINT('Ctrl Pts',(0.841298510752801,-0.0476299999999999,
0.504455939115715));
#9379=CARTESIAN_POINT('',(0.528110872004958,-0.04763,0.871530771444223));
#9380=CARTESIAN_POINT('Origin',(0.707106781186547,-0.04763,0.707106781186548));
#9381=CARTESIAN_POINT('',(0.871530771444223,-0.04763,0.528110872004959));
#9382=CARTESIAN_POINT('Ctrl Pts',(0.871530771444223,-0.0476300000000001,
0.528110872004958));
#9383=CARTESIAN_POINT('Ctrl Pts',(0.87014664509073,-0.0609922781173483,
0.530395067942936));
#9384=CARTESIAN_POINT('Ctrl Pts',(0.868149331745851,-0.0742967091364493,
0.533674141594226));
#9385=CARTESIAN_POINT('Ctrl Pts',(0.85981294420286,-0.115492077056649,0.54708917182331));
#9386=CARTESIAN_POINT('Ctrl Pts',(0.850993704737257,-0.141695629206859,
0.560922177770136));
#9387=CARTESIAN_POINT('Ctrl Pts',(0.830754510485543,-0.181890537957859,
0.590422647829571));
#9388=CARTESIAN_POINT('Ctrl Pts',(0.816896541396381,-0.201072148666545,
0.609616703125488));
#9389=CARTESIAN_POINT('Ctrl Pts',(0.792310597819928,-0.223955109275652,
0.641117951819998));
#9390=CARTESIAN_POINT('Ctrl Pts',(0.779109323683612,-0.232742381310829,
0.657208095763053));
#9391=CARTESIAN_POINT('Ctrl Pts',(0.750552691816206,-0.244234834628584,
0.68964083160521));
#9392=CARTESIAN_POINT('Ctrl Pts',(0.735185187071673,-0.246942143572133,
0.705971972091755));
#9393=CARTESIAN_POINT('Ctrl Pts',(0.705971972091754,-0.246942143572133,
0.735185187071673));
#9394=CARTESIAN_POINT('Ctrl Pts',(0.689640831605209,-0.244234834628584,
0.750552691816206));
#9395=CARTESIAN_POINT('Ctrl Pts',(0.657208095763052,-0.232742381310829,
0.779109323683612));
#9396=CARTESIAN_POINT('Ctrl Pts',(0.641117951819998,-0.223955109275652,
0.792310597819928));
#9397=CARTESIAN_POINT('Ctrl Pts',(0.609616703125487,-0.201072148666545,
0.816896541396382));
#9398=CARTESIAN_POINT('Ctrl Pts',(0.590422647829571,-0.181890537957858,
0.830754510485544));
#9399=CARTESIAN_POINT('Ctrl Pts',(0.560922177770135,-0.141695629206858,
0.850993704737257));
#9400=CARTESIAN_POINT('Ctrl Pts',(0.547089171823309,-0.115492077056649,
0.859812944202861));
#9401=CARTESIAN_POINT('Ctrl Pts',(0.533674141594226,-0.0742967091364491,
0.868149331745852));
#9402=CARTESIAN_POINT('Ctrl Pts',(0.530395067942936,-0.0609922781173483,
0.870146645090731));
#9403=CARTESIAN_POINT('Ctrl Pts',(0.528110872004958,-0.0476300000000001,
0.871530771444223));
#9404=CARTESIAN_POINT('Origin',(0.707106781186547,-0.04763,0.707106781186548));
#9405=CARTESIAN_POINT('Origin',(0.,-0.166705,0.));
#9406=CARTESIAN_POINT('',(0.242834539687906,-0.04763,0.989696097314));
#9407=CARTESIAN_POINT('Origin',(0.,-0.04763,0.));
#9408=CARTESIAN_POINT('',(-0.242834539687907,-0.04763,0.989696097314));
#9409=CARTESIAN_POINT('Ctrl Pts',(0.242834539687906,-0.04763,0.989696097314));
#9410=CARTESIAN_POINT('Ctrl Pts',(0.24024064412003,-0.0609922781173483,
0.990332542620729));
#9411=CARTESIAN_POINT('Ctrl Pts',(0.236509675094874,-0.0742967091364492,
0.991238884025248));
#9412=CARTESIAN_POINT('Ctrl Pts',(0.221129100087819,-0.115492077056649,
0.994830026707808));
#9413=CARTESIAN_POINT('Ctrl Pts',(0.205111543747588,-0.141695629206859,
0.998375294985966));
#9414=CARTESIAN_POINT('Ctrl Pts',(0.169940289819232,-0.181890537957859,
1.00492400591205));
#9415=CARTESIAN_POINT('Ctrl Pts',(0.1465689792446,-0.201072148666545,1.00869718865384));
#9416=CARTESIAN_POINT('Ctrl Pts',(0.106909345252087,-0.223955109275652,
1.01358704779679));
#9417=CARTESIAN_POINT('Ctrl Pts',(0.0861971848975941,-0.232742381310829,
1.0156297872271));
#9418=CARTESIAN_POINT('Ctrl Pts',(0.0430711894098822,-0.244234834628584,
1.01837060663223));
#9419=CARTESIAN_POINT('Ctrl Pts',(0.0206568624125605,-0.246942143572133,
1.019052));
#9420=CARTESIAN_POINT('Ctrl Pts',(-0.0206568624125608,-0.246942143572133,
1.019052));
#9421=CARTESIAN_POINT('Ctrl Pts',(-0.0430711894098825,-0.244234834628584,
1.01837060663223));
#9422=CARTESIAN_POINT('Ctrl Pts',(-0.0861971848975943,-0.232742381310829,
1.0156297872271));
#9423=CARTESIAN_POINT('Ctrl Pts',(-0.106909345252088,-0.223955109275652,
1.01358704779679));
#9424=CARTESIAN_POINT('Ctrl Pts',(-0.1465689792446,-0.201072148666545,1.00869718865384));
#9425=CARTESIAN_POINT('Ctrl Pts',(-0.169940289819232,-0.181890537957859,
1.00492400591205));
#9426=CARTESIAN_POINT('Ctrl Pts',(-0.205111543747588,-0.141695629206859,
0.998375294985966));
#9427=CARTESIAN_POINT('Ctrl Pts',(-0.221129100087819,-0.115492077056649,
0.994830026707808));
#9428=CARTESIAN_POINT('Ctrl Pts',(-0.236509675094875,-0.0742967091364493,
0.991238884025248));
#9429=CARTESIAN_POINT('Ctrl Pts',(-0.24024064412003,-0.0609922781173483,
0.990332542620729));
#9430=CARTESIAN_POINT('Ctrl Pts',(-0.242834539687907,-0.04763,0.989696097314));
#9431=CARTESIAN_POINT('',(-0.528110872004959,-0.04763,0.871530771444223));
#9432=CARTESIAN_POINT('Origin',(0.,-0.04763,0.));
#9433=CARTESIAN_POINT('',(-0.871530771444223,-0.04763,0.528110872004958));
#9434=CARTESIAN_POINT('Ctrl Pts',(-0.528110872004958,-0.0476300000000001,
0.871530771444223));
#9435=CARTESIAN_POINT('Ctrl Pts',(-0.530395067942936,-0.0609922781173484,
0.87014664509073));
#9436=CARTESIAN_POINT('Ctrl Pts',(-0.533674141594226,-0.0742967091364493,
0.868149331745851));
#9437=CARTESIAN_POINT('Ctrl Pts',(-0.54708917182331,-0.115492077056649,
0.85981294420286));
#9438=CARTESIAN_POINT('Ctrl Pts',(-0.560922177770136,-0.141695629206859,
0.850993704737257));
#9439=CARTESIAN_POINT('Ctrl Pts',(-0.590422647829571,-0.181890537957859,
0.830754510485543));
#9440=CARTESIAN_POINT('Ctrl Pts',(-0.609616703125488,-0.201072148666545,
0.816896541396381));
#9441=CARTESIAN_POINT('Ctrl Pts',(-0.641117951819998,-0.223955109275652,
0.792310597819928));
#9442=CARTESIAN_POINT('Ctrl Pts',(-0.657208095763053,-0.232742381310829,
0.779109323683611));
#9443=CARTESIAN_POINT('Ctrl Pts',(-0.68964083160521,-0.244234834628584,
0.750552691816205));
#9444=CARTESIAN_POINT('Ctrl Pts',(-0.705971972091755,-0.246942143572133,
0.735185187071673));
#9445=CARTESIAN_POINT('Ctrl Pts',(-0.735185187071673,-0.246942143572133,
0.705971972091754));
#9446=CARTESIAN_POINT('Ctrl Pts',(-0.750552691816206,-0.244234834628584,
0.689640831605209));
#9447=CARTESIAN_POINT('Ctrl Pts',(-0.779109323683612,-0.232742381310829,
0.657208095763052));
#9448=CARTESIAN_POINT('Ctrl Pts',(-0.792310597819928,-0.223955109275652,
0.641117951819998));
#9449=CARTESIAN_POINT('Ctrl Pts',(-0.816896541396382,-0.201072148666545,
0.609616703125487));
#9450=CARTESIAN_POINT('Ctrl Pts',(-0.830754510485544,-0.181890537957858,
0.590422647829571));
#9451=CARTESIAN_POINT('Ctrl Pts',(-0.850993704737257,-0.141695629206858,
0.560922177770135));
#9452=CARTESIAN_POINT('Ctrl Pts',(-0.859812944202861,-0.115492077056649,
0.547089171823309));
#9453=CARTESIAN_POINT('Ctrl Pts',(-0.868149331745852,-0.0742967091364491,
0.533674141594226));
#9454=CARTESIAN_POINT('Ctrl Pts',(-0.870146645090731,-0.0609922781173483,
0.530395067942936));
#9455=CARTESIAN_POINT('Ctrl Pts',(-0.871530771444223,-0.04763,0.528110872004958));
#9456=CARTESIAN_POINT('',(-0.989696097314,-0.04763,0.242834539687906));
#9457=CARTESIAN_POINT('Origin',(0.,-0.04763,0.));
#9458=CARTESIAN_POINT('',(-1.019052,-0.246942143572133,1.248489836334E-16));
#9459=CARTESIAN_POINT('Ctrl Pts',(-0.989696097314,-0.04763,0.242834539687906));
#9460=CARTESIAN_POINT('Ctrl Pts',(-0.990332542620729,-0.0609922781173483,
0.24024064412003));
#9461=CARTESIAN_POINT('Ctrl Pts',(-0.991238884025248,-0.0742967091364492,
0.236509675094874));
#9462=CARTESIAN_POINT('Ctrl Pts',(-0.994830026707808,-0.115492077056649,
0.221129100087819));
#9463=CARTESIAN_POINT('Ctrl Pts',(-0.998375294985966,-0.141695629206859,
0.205111543747588));
#9464=CARTESIAN_POINT('Ctrl Pts',(-1.00492400591205,-0.181890537957859,
0.169940289819232));
#9465=CARTESIAN_POINT('Ctrl Pts',(-1.00869718865384,-0.201072148666545,
0.1465689792446));
#9466=CARTESIAN_POINT('Ctrl Pts',(-1.01358704779679,-0.223955109275652,
0.106909345252088));
#9467=CARTESIAN_POINT('Ctrl Pts',(-1.0156297872271,-0.232742381310829,0.0861971848975944));
#9468=CARTESIAN_POINT('Ctrl Pts',(-1.01837060663223,-0.244234834628584,
0.0430711894098825));
#9469=CARTESIAN_POINT('Ctrl Pts',(-1.019052,-0.246942143572133,0.0206568624125608));
#9470=CARTESIAN_POINT('Ctrl Pts',(-1.019052,-0.246942143572133,1.2490009027033E-16));
#9471=CARTESIAN_POINT('',(-1.019052,-0.28578,1.24797876996471E-16));
#9472=CARTESIAN_POINT('',(-1.019052,-0.166705,1.24797876996471E-16));
#9473=CARTESIAN_POINT('Origin',(0.,-0.28578,0.));
#9474=CARTESIAN_POINT('',(-0.989696097314,-0.04763,-0.242834539687906));
#9475=CARTESIAN_POINT('Ctrl Pts',(-1.019052,-0.246942143572133,1.2490009027033E-16));
#9476=CARTESIAN_POINT('Ctrl Pts',(-1.019052,-0.246942143572133,-0.0206568624125605));
#9477=CARTESIAN_POINT('Ctrl Pts',(-1.01837060663223,-0.244234834628584,
-0.0430711894098822));
#9478=CARTESIAN_POINT('Ctrl Pts',(-1.0156297872271,-0.232742381310829,-0.0861971848975941));
#9479=CARTESIAN_POINT('Ctrl Pts',(-1.01358704779679,-0.223955109275652,
-0.106909345252087));
#9480=CARTESIAN_POINT('Ctrl Pts',(-1.00869718865384,-0.201072148666546,
-0.1465689792446));
#9481=CARTESIAN_POINT('Ctrl Pts',(-1.00492400591205,-0.181890537957859,
-0.169940289819232));
#9482=CARTESIAN_POINT('Ctrl Pts',(-0.998375294985966,-0.141695629206859,
-0.205111543747588));
#9483=CARTESIAN_POINT('Ctrl Pts',(-0.994830026707808,-0.11549207705665,
-0.221129100087819));
#9484=CARTESIAN_POINT('Ctrl Pts',(-0.991238884025248,-0.0742967091364495,
-0.236509675094874));
#9485=CARTESIAN_POINT('Ctrl Pts',(-0.990332542620729,-0.0609922781173484,
-0.24024064412003));
#9486=CARTESIAN_POINT('Ctrl Pts',(-0.989696097314,-0.0476300000000001,-0.242834539687907));
#9487=CARTESIAN_POINT('',(-0.871530771444223,-0.04763,-0.528110872004958));
#9488=CARTESIAN_POINT('Origin',(0.,-0.04763,0.));
#9489=CARTESIAN_POINT('',(-0.528110872004958,-0.04763,-0.871530771444223));
#9490=CARTESIAN_POINT('Ctrl Pts',(-0.871530771444223,-0.0476300000000001,
-0.528110872004958));
#9491=CARTESIAN_POINT('Ctrl Pts',(-0.87014664509073,-0.0609922781173484,
-0.530395067942936));
#9492=CARTESIAN_POINT('Ctrl Pts',(-0.868149331745851,-0.0742967091364494,
-0.533674141594226));
#9493=CARTESIAN_POINT('Ctrl Pts',(-0.85981294420286,-0.115492077056649,
-0.54708917182331));
#9494=CARTESIAN_POINT('Ctrl Pts',(-0.850993704737257,-0.141695629206859,
-0.560922177770136));
#9495=CARTESIAN_POINT('Ctrl Pts',(-0.830754510485543,-0.181890537957859,
-0.590422647829571));
#9496=CARTESIAN_POINT('Ctrl Pts',(-0.816896541396381,-0.201072148666546,
-0.609616703125488));
#9497=CARTESIAN_POINT('Ctrl Pts',(-0.792310597819928,-0.223955109275652,
-0.641117951819999));
#9498=CARTESIAN_POINT('Ctrl Pts',(-0.779109323683611,-0.232742381310829,
-0.657208095763053));
#9499=CARTESIAN_POINT('Ctrl Pts',(-0.750552691816205,-0.244234834628584,
-0.68964083160521));
#9500=CARTESIAN_POINT('Ctrl Pts',(-0.735185187071673,-0.246942143572133,
-0.705971972091755));
#9501=CARTESIAN_POINT('Ctrl Pts',(-0.705971972091754,-0.246942143572133,
-0.735185187071673));
#9502=CARTESIAN_POINT('Ctrl Pts',(-0.68964083160521,-0.244234834628584,
-0.750552691816206));
#9503=CARTESIAN_POINT('Ctrl Pts',(-0.657208095763052,-0.232742381310829,
-0.779109323683612));
#9504=CARTESIAN_POINT('Ctrl Pts',(-0.641117951819998,-0.223955109275652,
-0.792310597819928));
#9505=CARTESIAN_POINT('Ctrl Pts',(-0.609616703125488,-0.201072148666545,
-0.816896541396381));
#9506=CARTESIAN_POINT('Ctrl Pts',(-0.590422647829571,-0.181890537957859,
-0.830754510485543));
#9507=CARTESIAN_POINT('Ctrl Pts',(-0.560922177770136,-0.141695629206859,
-0.850993704737257));
#9508=CARTESIAN_POINT('Ctrl Pts',(-0.54708917182331,-0.115492077056649,
-0.85981294420286));
#9509=CARTESIAN_POINT('Ctrl Pts',(-0.533674141594226,-0.0742967091364494,
-0.868149331745852));
#9510=CARTESIAN_POINT('Ctrl Pts',(-0.530395067942936,-0.0609922781173484,
-0.870146645090731));
#9511=CARTESIAN_POINT('Ctrl Pts',(-0.528110872004958,-0.0476300000000001,
-0.871530771444223));
#9512=CARTESIAN_POINT('',(-0.242834539687906,-0.04763,-0.989696097314));
#9513=CARTESIAN_POINT('Origin',(0.,-0.04763,0.));
#9514=CARTESIAN_POINT('',(0.242834539687906,-0.04763,-0.989696097314));
#9515=CARTESIAN_POINT('Ctrl Pts',(-0.242834539687907,-0.04763,-0.989696097314));
#9516=CARTESIAN_POINT('Ctrl Pts',(-0.24024064412003,-0.0609922781173483,
-0.990332542620729));
#9517=CARTESIAN_POINT('Ctrl Pts',(-0.236509675094874,-0.0742967091364493,
-0.991238884025248));
#9518=CARTESIAN_POINT('Ctrl Pts',(-0.221129100087819,-0.115492077056649,
-0.994830026707808));
#9519=CARTESIAN_POINT('Ctrl Pts',(-0.205111543747588,-0.141695629206859,
-0.998375294985966));
#9520=CARTESIAN_POINT('Ctrl Pts',(-0.169940289819232,-0.181890537957859,
-1.00492400591205));
#9521=CARTESIAN_POINT('Ctrl Pts',(-0.1465689792446,-0.201072148666545,-1.00869718865384));
#9522=CARTESIAN_POINT('Ctrl Pts',(-0.106909345252087,-0.223955109275652,
-1.01358704779679));
#9523=CARTESIAN_POINT('Ctrl Pts',(-0.0861971848975942,-0.232742381310829,
-1.0156297872271));
#9524=CARTESIAN_POINT('Ctrl Pts',(-0.0430711894098823,-0.244234834628584,
-1.01837060663223));
#9525=CARTESIAN_POINT('Ctrl Pts',(-0.0206568624125606,-0.246942143572133,
-1.019052));
#9526=CARTESIAN_POINT('Ctrl Pts',(0.0206568624125607,-0.246942143572133,
-1.019052));
#9527=CARTESIAN_POINT('Ctrl Pts',(0.0430711894098824,-0.244234834628584,
-1.01837060663223));
#9528=CARTESIAN_POINT('Ctrl Pts',(0.0861971848975943,-0.232742381310829,
-1.0156297872271));
#9529=CARTESIAN_POINT('Ctrl Pts',(0.106909345252088,-0.223955109275652,
-1.01358704779679));
#9530=CARTESIAN_POINT('Ctrl Pts',(0.1465689792446,-0.201072148666545,-1.00869718865384));
#9531=CARTESIAN_POINT('Ctrl Pts',(0.169940289819232,-0.181890537957859,
-1.00492400591205));
#9532=CARTESIAN_POINT('Ctrl Pts',(0.205111543747588,-0.141695629206859,
-0.998375294985966));
#9533=CARTESIAN_POINT('Ctrl Pts',(0.221129100087819,-0.115492077056649,
-0.994830026707808));
#9534=CARTESIAN_POINT('Ctrl Pts',(0.236509675094874,-0.0742967091364493,
-0.991238884025248));
#9535=CARTESIAN_POINT('Ctrl Pts',(0.24024064412003,-0.0609922781173484,
-0.990332542620729));
#9536=CARTESIAN_POINT('Ctrl Pts',(0.242834539687907,-0.04763,-0.989696097314));
#9537=CARTESIAN_POINT('',(0.528110872004958,-0.04763,-0.871530771444223));
#9538=CARTESIAN_POINT('Origin',(0.,-0.04763,0.));
#9539=CARTESIAN_POINT('',(0.871530771444223,-0.04763,-0.528110872004958));
#9540=CARTESIAN_POINT('Ctrl Pts',(0.528110872004958,-0.0476300000000001,
-0.871530771444223));
#9541=CARTESIAN_POINT('Ctrl Pts',(0.530395067942936,-0.0609922781173484,
-0.870146645090731));
#9542=CARTESIAN_POINT('Ctrl Pts',(0.533674141594226,-0.0742967091364493,
-0.868149331745851));
#9543=CARTESIAN_POINT('Ctrl Pts',(0.54708917182331,-0.115492077056649,-0.85981294420286));
#9544=CARTESIAN_POINT('Ctrl Pts',(0.560922177770136,-0.141695629206859,
-0.850993704737257));
#9545=CARTESIAN_POINT('Ctrl Pts',(0.590422647829571,-0.181890537957859,
-0.830754510485543));
#9546=CARTESIAN_POINT('Ctrl Pts',(0.609616703125488,-0.201072148666545,
-0.816896541396381));
#9547=CARTESIAN_POINT('Ctrl Pts',(0.641117951819998,-0.223955109275652,
-0.792310597819928));
#9548=CARTESIAN_POINT('Ctrl Pts',(0.657208095763053,-0.232742381310829,
-0.779109323683612));
#9549=CARTESIAN_POINT('Ctrl Pts',(0.68964083160521,-0.244234834628584,-0.750552691816206));
#9550=CARTESIAN_POINT('Ctrl Pts',(0.705971972091755,-0.246942143572133,
-0.735185187071673));
#9551=CARTESIAN_POINT('Ctrl Pts',(0.735185187071673,-0.246942143572133,
-0.705971972091754));
#9552=CARTESIAN_POINT('Ctrl Pts',(0.750552691816206,-0.244234834628584,
-0.68964083160521));
#9553=CARTESIAN_POINT('Ctrl Pts',(0.779109323683612,-0.232742381310829,
-0.657208095763053));
#9554=CARTESIAN_POINT('Ctrl Pts',(0.792310597819928,-0.223955109275652,
-0.641117951819998));
#9555=CARTESIAN_POINT('Ctrl Pts',(0.816896541396381,-0.201072148666545,
-0.609616703125488));
#9556=CARTESIAN_POINT('Ctrl Pts',(0.830754510485543,-0.181890537957859,
-0.590422647829571));
#9557=CARTESIAN_POINT('Ctrl Pts',(0.850993704737257,-0.141695629206859,
-0.560922177770136));
#9558=CARTESIAN_POINT('Ctrl Pts',(0.85981294420286,-0.115492077056649,-0.54708917182331));
#9559=CARTESIAN_POINT('Ctrl Pts',(0.868149331745851,-0.0742967091364493,
-0.533674141594226));
#9560=CARTESIAN_POINT('Ctrl Pts',(0.870146645090731,-0.0609922781173484,
-0.530395067942936));
#9561=CARTESIAN_POINT('Ctrl Pts',(0.871530771444223,-0.0476300000000001,
-0.528110872004958));
#9562=CARTESIAN_POINT('',(0.989696097314,-0.04763,-0.242834539687906));
#9563=CARTESIAN_POINT('Origin',(0.,-0.04763,0.));
#9564=CARTESIAN_POINT('',(0.989696097314,-0.04763,0.242834539687906));
#9565=CARTESIAN_POINT('Ctrl Pts',(0.989696097314,-0.04763,-0.242834539687907));
#9566=CARTESIAN_POINT('Ctrl Pts',(0.990332542620729,-0.0609922781173483,
-0.24024064412003));
#9567=CARTESIAN_POINT('Ctrl Pts',(0.991238884025248,-0.0742967091364493,
-0.236509675094874));
#9568=CARTESIAN_POINT('Ctrl Pts',(0.994830026707808,-0.115492077056649,
-0.221129100087819));
#9569=CARTESIAN_POINT('Ctrl Pts',(0.998375294985966,-0.141695629206859,
-0.205111543747588));
#9570=CARTESIAN_POINT('Ctrl Pts',(1.00492400591205,-0.181890537957859,-0.169940289819232));
#9571=CARTESIAN_POINT('Ctrl Pts',(1.00869718865384,-0.201072148666545,-0.1465689792446));
#9572=CARTESIAN_POINT('Ctrl Pts',(1.01358704779679,-0.223955109275652,-0.106909345252087));
#9573=CARTESIAN_POINT('Ctrl Pts',(1.0156297872271,-0.232742381310829,-0.0861971848975942));
#9574=CARTESIAN_POINT('Ctrl Pts',(1.01837060663223,-0.244234834628584,-0.0430711894098823));
#9575=CARTESIAN_POINT('Ctrl Pts',(1.019052,-0.246942143572133,-0.0206568624125607));
#9576=CARTESIAN_POINT('Ctrl Pts',(1.019052,-0.246942143572133,0.0206568624125607));
#9577=CARTESIAN_POINT('Ctrl Pts',(1.01837060663223,-0.244234834628584,0.0430711894098823));
#9578=CARTESIAN_POINT('Ctrl Pts',(1.0156297872271,-0.232742381310829,0.0861971848975942));
#9579=CARTESIAN_POINT('Ctrl Pts',(1.01358704779679,-0.223955109275652,0.106909345252087));
#9580=CARTESIAN_POINT('Ctrl Pts',(1.00869718865384,-0.201072148666545,0.1465689792446));
#9581=CARTESIAN_POINT('Ctrl Pts',(1.00492400591205,-0.181890537957859,0.169940289819232));
#9582=CARTESIAN_POINT('Ctrl Pts',(0.998375294985966,-0.141695629206859,
0.205111543747588));
#9583=CARTESIAN_POINT('Ctrl Pts',(0.994830026707808,-0.115492077056649,
0.221129100087819));
#9584=CARTESIAN_POINT('Ctrl Pts',(0.991238884025248,-0.0742967091364492,
0.236509675094874));
#9585=CARTESIAN_POINT('Ctrl Pts',(0.990332542620729,-0.0609922781173483,
0.24024064412003));
#9586=CARTESIAN_POINT('Ctrl Pts',(0.989696097314,-0.04763,0.242834539687907));
#9587=CARTESIAN_POINT('Origin',(0.,-0.04763,0.));
#9588=CARTESIAN_POINT('Origin',(0.,-0.04763,0.));
#9589=CARTESIAN_POINT('',(0.238183666596899,-0.04763,0.951592097314));
#9590=CARTESIAN_POINT('Origin',(0.,-0.04763,0.));
#9591=CARTESIAN_POINT('Origin',(-1.94289029309402E-16,-0.04763,1.));
#9592=CARTESIAN_POINT('Origin',(-1.94289029309402E-16,0.,1.));
#9593=CARTESIAN_POINT('',(-0.2381836665969,-0.04763,0.951592097314));
#9594=CARTESIAN_POINT('Ctrl Pts',(-0.238183666596899,-0.0476299999999999,
0.951592097314));
#9595=CARTESIAN_POINT('Ctrl Pts',(-0.233157223576062,-0.0740444353928835,
0.952850216871763));
#9596=CARTESIAN_POINT('Ctrl Pts',(-0.223801617934946,-0.0999305678883309,
0.955173119738174));
#9597=CARTESIAN_POINT('Ctrl Pts',(-0.199966927975188,-0.142345102874864,
0.960411259488514));
#9598=CARTESIAN_POINT('Ctrl Pts',(-0.1868781821531,-0.159766064500479,0.963103647174702));
#9599=CARTESIAN_POINT('Ctrl Pts',(-0.15681442133453,-0.190326085855194,
0.968453058988463));
#9600=CARTESIAN_POINT('Ctrl Pts',(-0.139836317888043,-0.203463743702801,
0.971100730005489));
#9601=CARTESIAN_POINT('Ctrl Pts',(-0.104422493053067,-0.224161999508995,
0.975530745318961));
#9602=CARTESIAN_POINT('Ctrl Pts',(-0.0842175114474176,-0.232861760990032,
0.977553872336861));
#9603=CARTESIAN_POINT('Ctrl Pts',(-0.0421062857595701,-0.244251601209411,
0.980270995488453));
#9604=CARTESIAN_POINT('Ctrl Pts',(-0.0201990724523197,-0.246942143572133,
0.980948));
#9605=CARTESIAN_POINT('Ctrl Pts',(0.020199072452319,-0.246942143572133,
0.980948));
#9606=CARTESIAN_POINT('Ctrl Pts',(0.0421062857595694,-0.244251601209411,
0.980270995488454));
#9607=CARTESIAN_POINT('Ctrl Pts',(0.0842175114474169,-0.232861760990032,
0.977553872336861));
#9608=CARTESIAN_POINT('Ctrl Pts',(0.104422493053067,-0.224161999508995,
0.975530745318961));
#9609=CARTESIAN_POINT('Ctrl Pts',(0.139836317888042,-0.203463743702801,
0.971100730005489));
#9610=CARTESIAN_POINT('Ctrl Pts',(0.15681442133453,-0.190326085855194,0.968453058988463));
#9611=CARTESIAN_POINT('Ctrl Pts',(0.1868781821531,-0.15976606450048,0.963103647174702));
#9612=CARTESIAN_POINT('Ctrl Pts',(0.199966927975188,-0.142345102874864,
0.960411259488514));
#9613=CARTESIAN_POINT('Ctrl Pts',(0.223801617934945,-0.0999305678883309,
0.955173119738174));
#9614=CARTESIAN_POINT('Ctrl Pts',(0.233157223576061,-0.0740444353928835,
0.952850216871763));
#9615=CARTESIAN_POINT('Ctrl Pts',(0.238183666596899,-0.0476299999999999,
0.951592097314));
#9616=CARTESIAN_POINT('Origin',(-1.94289029309402E-16,-0.04763,1.));
#9617=CARTESIAN_POINT('Origin',(0.,-0.04763,0.));
#9618=CARTESIAN_POINT('',(-0.504455939115715,-0.04763,0.841298510752802));
#9619=CARTESIAN_POINT('Origin',(0.,-0.04763,0.));
#9620=CARTESIAN_POINT('Origin',(-0.707106781186548,-0.04763,0.707106781186547));
#9621=CARTESIAN_POINT('Origin',(-0.707106781186548,0.,0.707106781186547));
#9622=CARTESIAN_POINT('',(-0.841298510752802,-0.04763,0.504455939115715));
#9623=CARTESIAN_POINT('Ctrl Pts',(-0.841298510752802,-0.04763,0.504455939115715));
#9624=CARTESIAN_POINT('Ctrl Pts',(-0.838633903678357,-0.0740444353928835,
0.508899795931835));
#9625=CARTESIAN_POINT('Ctrl Pts',(-0.833661031856294,-0.0999305678883309,
0.517157748491652));
#9626=CARTESIAN_POINT('Ctrl Pts',(-0.820511285096538,-0.142345102874864,
0.537715343527944));
#9627=CARTESIAN_POINT('Ctrl Pts',(-0.813159949759,-0.159766064500479,0.548874290046456));
#9628=CARTESIAN_POINT('Ctrl Pts',(-0.795684265985089,-0.190326085855194,
0.573915184558107));
#9629=CARTESIAN_POINT('Ctrl Pts',(-0.78555112003688,-0.203463743702801,
0.587792702767295));
#9630=CARTESIAN_POINT('Ctrl Pts',(-0.763642258217233,-0.224161999508995,
0.615966552324775));
#9631=CARTESIAN_POINT('Ctrl Pts',(-0.750785745543687,-0.232861760990032,
0.631684198665438));
#9632=CARTESIAN_POINT('Ctrl Pts',(-0.722929908501543,-0.244251601209411,
0.663382628119203));
#9633=CARTESIAN_POINT('Ctrl Pts',(-0.707917883896095,-0.246942143572133,
0.679352081686668));
#9634=CARTESIAN_POINT('Ctrl Pts',(-0.679352081686668,-0.246942143572133,
0.707917883896095));
#9635=CARTESIAN_POINT('Ctrl Pts',(-0.663382628119203,-0.244251601209411,
0.722929908501544));
#9636=CARTESIAN_POINT('Ctrl Pts',(-0.631684198665438,-0.232861760990031,
0.750785745543687));
#9637=CARTESIAN_POINT('Ctrl Pts',(-0.615966552324775,-0.224161999508995,
0.763642258217233));
#9638=CARTESIAN_POINT('Ctrl Pts',(-0.587792702767295,-0.203463743702801,
0.78555112003688));
#9639=CARTESIAN_POINT('Ctrl Pts',(-0.573915184558107,-0.190326085855194,
0.795684265985088));
#9640=CARTESIAN_POINT('Ctrl Pts',(-0.548874290046456,-0.159766064500479,
0.813159949759));
#9641=CARTESIAN_POINT('Ctrl Pts',(-0.537715343527944,-0.142345102874864,
0.820511285096538));
#9642=CARTESIAN_POINT('Ctrl Pts',(-0.517157748491652,-0.0999305678883309,
0.833661031856294));
#9643=CARTESIAN_POINT('Ctrl Pts',(-0.508899795931835,-0.0740444353928835,
0.838633903678357));
#9644=CARTESIAN_POINT('Ctrl Pts',(-0.504455939115716,-0.04763,0.841298510752801));
#9645=CARTESIAN_POINT('Origin',(-0.707106781186548,-0.04763,0.707106781186547));
#9646=CARTESIAN_POINT('Origin',(0.,-0.04763,0.));
#9647=CARTESIAN_POINT('',(-0.951592097314,-0.04763,0.238183666596899));
#9648=CARTESIAN_POINT('Origin',(0.,-0.04763,0.));
#9649=CARTESIAN_POINT('Origin',(-1.,-0.04763,-1.11022302462516E-16));
#9650=CARTESIAN_POINT('Origin',(-1.,0.,-1.11022302462516E-16));
#9651=CARTESIAN_POINT('',(-0.951592097314,-0.04763,-0.2381836665969));
#9652=CARTESIAN_POINT('',(-0.980948,-0.246942143572133,1.08514323328844E-18));
#9653=CARTESIAN_POINT('Ctrl Pts',(-0.951592097314,-0.04763,-0.238183666596899));
#9654=CARTESIAN_POINT('Ctrl Pts',(-0.952850216871763,-0.0740444353928835,
-0.233157223576062));
#9655=CARTESIAN_POINT('Ctrl Pts',(-0.955173119738174,-0.0999305678883309,
-0.223801617934946));
#9656=CARTESIAN_POINT('Ctrl Pts',(-0.960411259488514,-0.142345102874864,
-0.199966927975188));
#9657=CARTESIAN_POINT('Ctrl Pts',(-0.963103647174702,-0.159766064500479,
-0.1868781821531));
#9658=CARTESIAN_POINT('Ctrl Pts',(-0.968453058988463,-0.190326085855194,
-0.15681442133453));
#9659=CARTESIAN_POINT('Ctrl Pts',(-0.971100730005489,-0.203463743702801,
-0.139836317888043));
#9660=CARTESIAN_POINT('Ctrl Pts',(-0.975530745318961,-0.224161999508995,
-0.104422493053067));
#9661=CARTESIAN_POINT('Ctrl Pts',(-0.977553872336861,-0.232861760990032,
-0.0842175114474175));
#9662=CARTESIAN_POINT('Ctrl Pts',(-0.980270995488453,-0.244251601209411,
-0.0421062857595699));
#9663=CARTESIAN_POINT('Ctrl Pts',(-0.980948,-0.246942143572133,-0.0201990724523195));
#9664=CARTESIAN_POINT('Ctrl Pts',(-0.980948,-0.246942143572133,-1.17961196366423E-16));
#9665=CARTESIAN_POINT('Origin',(-1.,-0.04763,-1.11022302462516E-16));
#9666=CARTESIAN_POINT('Ctrl Pts',(-0.980948,-0.246942143572133,-1.17961196366423E-16));
#9667=CARTESIAN_POINT('Ctrl Pts',(-0.980948,-0.246942143572133,0.0201990724523192));
#9668=CARTESIAN_POINT('Ctrl Pts',(-0.980270995488453,-0.244251601209411,
0.0421062857595695));
#9669=CARTESIAN_POINT('Ctrl Pts',(-0.977553872336861,-0.232861760990032,
0.0842175114474169));
#9670=CARTESIAN_POINT('Ctrl Pts',(-0.975530745318961,-0.224161999508995,
0.104422493053066));
#9671=CARTESIAN_POINT('Ctrl Pts',(-0.971100730005489,-0.203463743702801,
0.139836317888042));
#9672=CARTESIAN_POINT('Ctrl Pts',(-0.968453058988463,-0.190326085855194,
0.15681442133453));
#9673=CARTESIAN_POINT('Ctrl Pts',(-0.963103647174702,-0.15976606450048,
0.1868781821531));
#9674=CARTESIAN_POINT('Ctrl Pts',(-0.960411259488514,-0.142345102874864,
0.199966927975188));
#9675=CARTESIAN_POINT('Ctrl Pts',(-0.955173119738174,-0.099930567888331,
0.223801617934945));
#9676=CARTESIAN_POINT('Ctrl Pts',(-0.952850216871763,-0.0740444353928835,
0.233157223576061));
#9677=CARTESIAN_POINT('Ctrl Pts',(-0.951592097314,-0.04763,0.238183666596899));
#9678=CARTESIAN_POINT('Origin',(0.,-0.04763,0.));
#9679=CARTESIAN_POINT('',(-0.841298510752802,-0.04763,-0.504455939115715));
#9680=CARTESIAN_POINT('Origin',(0.,-0.04763,0.));
#9681=CARTESIAN_POINT('Origin',(-0.707106781186547,-0.04763,-0.707106781186548));
#9682=CARTESIAN_POINT('Origin',(-0.707106781186547,0.,-0.707106781186548));
#9683=CARTESIAN_POINT('',(-0.504455939115715,-0.04763,-0.841298510752802));
#9684=CARTESIAN_POINT('Ctrl Pts',(-0.504455939115715,-0.04763,-0.841298510752802));
#9685=CARTESIAN_POINT('Ctrl Pts',(-0.508899795931835,-0.0740444353928835,
-0.838633903678357));
#9686=CARTESIAN_POINT('Ctrl Pts',(-0.517157748491652,-0.0999305678883309,
-0.833661031856294));
#9687=CARTESIAN_POINT('Ctrl Pts',(-0.537715343527944,-0.142345102874864,
-0.820511285096538));
#9688=CARTESIAN_POINT('Ctrl Pts',(-0.548874290046456,-0.159766064500479,
-0.813159949759));
#9689=CARTESIAN_POINT('Ctrl Pts',(-0.573915184558107,-0.190326085855194,
-0.795684265985089));
#9690=CARTESIAN_POINT('Ctrl Pts',(-0.587792702767295,-0.203463743702801,
-0.78555112003688));
#9691=CARTESIAN_POINT('Ctrl Pts',(-0.615966552324775,-0.224161999508995,
-0.763642258217233));
#9692=CARTESIAN_POINT('Ctrl Pts',(-0.631684198665438,-0.232861760990032,
-0.750785745543687));
#9693=CARTESIAN_POINT('Ctrl Pts',(-0.663382628119203,-0.244251601209411,
-0.722929908501543));
#9694=CARTESIAN_POINT('Ctrl Pts',(-0.679352081686668,-0.246942143572133,
-0.707917883896095));
#9695=CARTESIAN_POINT('Ctrl Pts',(-0.707917883896095,-0.246942143572133,
-0.679352081686668));
#9696=CARTESIAN_POINT('Ctrl Pts',(-0.722929908501543,-0.244251601209411,
-0.663382628119203));
#9697=CARTESIAN_POINT('Ctrl Pts',(-0.750785745543687,-0.232861760990032,
-0.631684198665439));
#9698=CARTESIAN_POINT('Ctrl Pts',(-0.763642258217232,-0.224161999508995,
-0.615966552324775));
#9699=CARTESIAN_POINT('Ctrl Pts',(-0.78555112003688,-0.203463743702801,
-0.587792702767295));
#9700=CARTESIAN_POINT('Ctrl Pts',(-0.795684265985088,-0.190326085855194,
-0.573915184558107));
#9701=CARTESIAN_POINT('Ctrl Pts',(-0.813159949759,-0.15976606450048,-0.548874290046456));
#9702=CARTESIAN_POINT('Ctrl Pts',(-0.820511285096538,-0.142345102874864,
-0.537715343527944));
#9703=CARTESIAN_POINT('Ctrl Pts',(-0.833661031856294,-0.0999305678883311,
-0.517157748491652));
#9704=CARTESIAN_POINT('Ctrl Pts',(-0.838633903678357,-0.0740444353928836,
-0.508899795931835));
#9705=CARTESIAN_POINT('Ctrl Pts',(-0.841298510752801,-0.04763,-0.504455939115715));
#9706=CARTESIAN_POINT('Origin',(-0.707106781186547,-0.04763,-0.707106781186548));
#9707=CARTESIAN_POINT('Origin',(0.,-0.04763,0.));
#9708=CARTESIAN_POINT('',(-0.238183666596899,-0.04763,-0.951592097314));
#9709=CARTESIAN_POINT('Origin',(0.,-0.04763,0.));
#9710=CARTESIAN_POINT('Origin',(5.55111512312578E-17,-0.04763,-1.));
#9711=CARTESIAN_POINT('Origin',(5.55111512312578E-17,0.,-1.));
#9712=CARTESIAN_POINT('',(0.238183666596899,-0.04763,-0.951592097314));
#9713=CARTESIAN_POINT('Ctrl Pts',(0.238183666596899,-0.04763,-0.951592097314));
#9714=CARTESIAN_POINT('Ctrl Pts',(0.233157223576062,-0.0740444353928835,
-0.952850216871763));
#9715=CARTESIAN_POINT('Ctrl Pts',(0.223801617934946,-0.099930567888331,
-0.955173119738174));
#9716=CARTESIAN_POINT('Ctrl Pts',(0.199966927975188,-0.142345102874864,
-0.960411259488514));
#9717=CARTESIAN_POINT('Ctrl Pts',(0.1868781821531,-0.15976606450048,-0.963103647174702));
#9718=CARTESIAN_POINT('Ctrl Pts',(0.15681442133453,-0.190326085855194,-0.968453058988463));
#9719=CARTESIAN_POINT('Ctrl Pts',(0.139836317888042,-0.203463743702801,
-0.971100730005489));
#9720=CARTESIAN_POINT('Ctrl Pts',(0.104422493053067,-0.224161999508995,
-0.975530745318961));
#9721=CARTESIAN_POINT('Ctrl Pts',(0.0842175114474173,-0.232861760990032,
-0.977553872336861));
#9722=CARTESIAN_POINT('Ctrl Pts',(0.0421062857595698,-0.244251601209411,
-0.980270995488453));
#9723=CARTESIAN_POINT('Ctrl Pts',(0.0201990724523194,-0.246942143572133,
-0.980948));
#9724=CARTESIAN_POINT('Ctrl Pts',(-0.0201990724523193,-0.246942143572133,
-0.980948));
#9725=CARTESIAN_POINT('Ctrl Pts',(-0.0421062857595697,-0.244251601209411,
-0.980270995488453));
#9726=CARTESIAN_POINT('Ctrl Pts',(-0.0842175114474171,-0.232861760990032,
-0.977553872336861));
#9727=CARTESIAN_POINT('Ctrl Pts',(-0.104422493053067,-0.224161999508995,
-0.975530745318961));
#9728=CARTESIAN_POINT('Ctrl Pts',(-0.139836317888042,-0.203463743702801,
-0.971100730005489));
#9729=CARTESIAN_POINT('Ctrl Pts',(-0.15681442133453,-0.190326085855194,
-0.968453058988463));
#9730=CARTESIAN_POINT('Ctrl Pts',(-0.1868781821531,-0.15976606450048,-0.963103647174702));
#9731=CARTESIAN_POINT('Ctrl Pts',(-0.199966927975188,-0.142345102874864,
-0.960411259488514));
#9732=CARTESIAN_POINT('Ctrl Pts',(-0.223801617934945,-0.099930567888331,
-0.955173119738174));
#9733=CARTESIAN_POINT('Ctrl Pts',(-0.233157223576062,-0.0740444353928835,
-0.952850216871763));
#9734=CARTESIAN_POINT('Ctrl Pts',(-0.238183666596899,-0.0476299999999999,
-0.951592097314));
#9735=CARTESIAN_POINT('Origin',(5.55111512312578E-17,-0.04763,-1.));
#9736=CARTESIAN_POINT('Origin',(0.,-0.04763,0.));
#9737=CARTESIAN_POINT('',(0.504455939115715,-0.04763,-0.841298510752802));
#9738=CARTESIAN_POINT('Origin',(0.,-0.04763,0.));
#9739=CARTESIAN_POINT('Origin',(0.707106781186548,-0.04763,-0.707106781186547));
#9740=CARTESIAN_POINT('Origin',(0.707106781186548,0.,-0.707106781186547));
#9741=CARTESIAN_POINT('',(0.841298510752802,-0.04763,-0.504455939115715));
#9742=CARTESIAN_POINT('Ctrl Pts',(0.841298510752802,-0.04763,-0.504455939115715));
#9743=CARTESIAN_POINT('Ctrl Pts',(0.838633903678357,-0.0740444353928835,
-0.508899795931835));
#9744=CARTESIAN_POINT('Ctrl Pts',(0.833661031856294,-0.0999305678883309,
-0.517157748491652));
#9745=CARTESIAN_POINT('Ctrl Pts',(0.820511285096538,-0.142345102874864,
-0.537715343527944));
#9746=CARTESIAN_POINT('Ctrl Pts',(0.813159949759,-0.159766064500479,-0.548874290046456));
#9747=CARTESIAN_POINT('Ctrl Pts',(0.795684265985088,-0.190326085855194,
-0.573915184558107));
#9748=CARTESIAN_POINT('Ctrl Pts',(0.78555112003688,-0.203463743702801,-0.587792702767295));
#9749=CARTESIAN_POINT('Ctrl Pts',(0.763642258217233,-0.224161999508995,
-0.615966552324775));
#9750=CARTESIAN_POINT('Ctrl Pts',(0.750785745543687,-0.232861760990032,
-0.631684198665438));
#9751=CARTESIAN_POINT('Ctrl Pts',(0.722929908501543,-0.244251601209411,
-0.663382628119203));
#9752=CARTESIAN_POINT('Ctrl Pts',(0.707917883896095,-0.246942143572133,
-0.679352081686668));
#9753=CARTESIAN_POINT('Ctrl Pts',(0.679352081686668,-0.246942143572133,
-0.707917883896095));
#9754=CARTESIAN_POINT('Ctrl Pts',(0.663382628119203,-0.244251601209411,
-0.722929908501543));
#9755=CARTESIAN_POINT('Ctrl Pts',(0.631684198665438,-0.232861760990032,
-0.750785745543687));
#9756=CARTESIAN_POINT('Ctrl Pts',(0.615966552324775,-0.224161999508995,
-0.763642258217232));
#9757=CARTESIAN_POINT('Ctrl Pts',(0.587792702767295,-0.203463743702801,
-0.78555112003688));
#9758=CARTESIAN_POINT('Ctrl Pts',(0.573915184558107,-0.190326085855194,
-0.795684265985088));
#9759=CARTESIAN_POINT('Ctrl Pts',(0.548874290046456,-0.159766064500479,
-0.813159949759));
#9760=CARTESIAN_POINT('Ctrl Pts',(0.537715343527944,-0.142345102874864,
-0.820511285096538));
#9761=CARTESIAN_POINT('Ctrl Pts',(0.517157748491652,-0.099930567888331,
-0.833661031856294));
#9762=CARTESIAN_POINT('Ctrl Pts',(0.508899795931835,-0.0740444353928835,
-0.838633903678357));
#9763=CARTESIAN_POINT('Ctrl Pts',(0.504455939115715,-0.04763,-0.841298510752801));
#9764=CARTESIAN_POINT('Origin',(0.707106781186548,-0.04763,-0.707106781186547));
#9765=CARTESIAN_POINT('Origin',(0.,-0.166705,0.));
#9766=CARTESIAN_POINT('',(-0.980948,-0.28578,1.20131482833E-16));
#9767=CARTESIAN_POINT('Origin',(0.,-0.28578,0.));
#9768=CARTESIAN_POINT('',(-0.980948,-0.166705,1.20131482833E-16));
#9769=CARTESIAN_POINT('',(0.951592097314,-0.04763,0.238183666596899));
#9770=CARTESIAN_POINT('Origin',(0.,-0.04763,0.));
#9771=CARTESIAN_POINT('',(0.951592097314,-0.04763,-0.238183666596899));
#9772=CARTESIAN_POINT('Ctrl Pts',(0.951592097314,-0.04763,0.238183666596899));
#9773=CARTESIAN_POINT('Ctrl Pts',(0.952850216871763,-0.0740444353928835,
0.233157223576062));
#9774=CARTESIAN_POINT('Ctrl Pts',(0.955173119738174,-0.099930567888331,
0.223801617934945));
#9775=CARTESIAN_POINT('Ctrl Pts',(0.960411259488514,-0.142345102874864,
0.199966927975188));
#9776=CARTESIAN_POINT('Ctrl Pts',(0.963103647174702,-0.15976606450048,0.1868781821531));
#9777=CARTESIAN_POINT('Ctrl Pts',(0.968453058988463,-0.190326085855194,
0.15681442133453));
#9778=CARTESIAN_POINT('Ctrl Pts',(0.971100730005489,-0.203463743702801,
0.139836317888042));
#9779=CARTESIAN_POINT('Ctrl Pts',(0.975530745318961,-0.224161999508995,
0.104422493053067));
#9780=CARTESIAN_POINT('Ctrl Pts',(0.977553872336861,-0.232861760990032,
0.0842175114474172));
#9781=CARTESIAN_POINT('Ctrl Pts',(0.980270995488453,-0.244251601209411,
0.0421062857595697));
#9782=CARTESIAN_POINT('Ctrl Pts',(0.980948,-0.246942143572133,0.0201990724523194));
#9783=CARTESIAN_POINT('Ctrl Pts',(0.980948,-0.246942143572133,-0.0201990724523194));
#9784=CARTESIAN_POINT('Ctrl Pts',(0.980270995488453,-0.244251601209411,
-0.0421062857595697));
#9785=CARTESIAN_POINT('Ctrl Pts',(0.977553872336861,-0.232861760990032,
-0.0842175114474172));
#9786=CARTESIAN_POINT('Ctrl Pts',(0.975530745318961,-0.224161999508995,
-0.104422493053067));
#9787=CARTESIAN_POINT('Ctrl Pts',(0.971100730005489,-0.203463743702801,
-0.139836317888042));
#9788=CARTESIAN_POINT('Ctrl Pts',(0.968453058988463,-0.190326085855194,
-0.15681442133453));
#9789=CARTESIAN_POINT('Ctrl Pts',(0.963103647174702,-0.15976606450048,-0.1868781821531));
#9790=CARTESIAN_POINT('Ctrl Pts',(0.960411259488514,-0.142345102874864,
-0.199966927975188));
#9791=CARTESIAN_POINT('Ctrl Pts',(0.955173119738174,-0.099930567888331,
-0.223801617934945));
#9792=CARTESIAN_POINT('Ctrl Pts',(0.952850216871763,-0.0740444353928835,
-0.233157223576062));
#9793=CARTESIAN_POINT('Ctrl Pts',(0.951592097314,-0.0476299999999999,-0.238183666596899));
#9794=CARTESIAN_POINT('Origin',(0.,-0.04763,0.));
#9795=CARTESIAN_POINT('Origin',(0.,-0.04763,0.));
#9796=CARTESIAN_POINT('Origin',(1.,-0.04763,0.));
#9797=CARTESIAN_POINT('Origin',(1.,0.,0.));
#9798=CARTESIAN_POINT('Origin',(1.,-0.04763,0.));
#9799=CARTESIAN_POINT('Origin',(0.,-0.28578,0.));
#9800=CARTESIAN_POINT('Origin',(0.,-0.04763,0.));
#9801=CARTESIAN_POINT('',(0.,0.,0.));
#9802=CARTESIAN_POINT('Origin',(1.013815,0.445,0.));
#9803=CARTESIAN_POINT('',(-1.013815,0.445,-1.24156529467757E-16));
#9804=CARTESIAN_POINT('Origin',(0.,0.445,0.));
#9805=CARTESIAN_POINT('',(-0.991185,0.445,-1.21385153761287E-16));
#9806=CARTESIAN_POINT('Origin',(0.,0.445,0.));
#9807=CARTESIAN_POINT('Origin',(0.,0.4075,0.));
#9808=CARTESIAN_POINT('',(-1.013815,0.37,-1.24156529467757E-16));
#9809=CARTESIAN_POINT('Origin',(0.,0.37,0.));
#9810=CARTESIAN_POINT('',(-1.013815,0.4075,-1.24156529467757E-16));
#9811=CARTESIAN_POINT('Origin',(0.991185,0.37,0.));
#9812=CARTESIAN_POINT('',(-0.991185,0.37,-1.21385153761287E-16));
#9813=CARTESIAN_POINT('Origin',(0.,0.37,0.));
#9814=CARTESIAN_POINT('Origin',(0.,0.4075,0.));
#9815=CARTESIAN_POINT('',(-0.991185,0.4075,-1.21385153761287E-16));
#9816=CARTESIAN_POINT('Origin',(1.013815,-0.37,0.));
#9817=CARTESIAN_POINT('',(-1.013815,-0.37,-1.24156529467757E-16));
#9818=CARTESIAN_POINT('Origin',(0.,-0.37,0.));
#9819=CARTESIAN_POINT('',(-0.991185,-0.37,-1.21385153761287E-16));
#9820=CARTESIAN_POINT('Origin',(0.,-0.37,0.));
#9821=CARTESIAN_POINT('Origin',(0.,-0.4075,0.));
#9822=CARTESIAN_POINT('',(-1.013815,-0.445,-1.24156529467757E-16));
#9823=CARTESIAN_POINT('Origin',(0.,-0.445,0.));
#9824=CARTESIAN_POINT('',(-1.013815,-0.4075,-1.24156529467757E-16));
#9825=CARTESIAN_POINT('Origin',(0.991185,-0.445,0.));
#9826=CARTESIAN_POINT('',(-0.991185,-0.445,-1.21385153761287E-16));
#9827=CARTESIAN_POINT('Origin',(0.,-0.445,0.));
#9828=CARTESIAN_POINT('Origin',(0.,-0.4075,0.));
#9829=CARTESIAN_POINT('',(-0.991185,-0.4075,-1.21385153761287E-16));
#9830=CARTESIAN_POINT('',(0.,0.,0.));
#9831=CARTESIAN_POINT('',(0.,0.,0.));
#9832=CARTESIAN_POINT('',(0.,0.,0.));
#9833=CARTESIAN_POINT('',(0.,0.,0.));
#9834=CARTESIAN_POINT('',(0.,0.,0.));
#9835=CARTESIAN_POINT('',(0.,0.,0.));
#9836=CARTESIAN_POINT('',(0.,0.,0.));
#9837=CARTESIAN_POINT('Origin',(0.,0.,5.9));
#9838=CARTESIAN_POINT('',(-0.165,-2.02066721859313E-17,5.9));
#9839=CARTESIAN_POINT('Origin',(0.,0.,5.9));
#9840=CARTESIAN_POINT('',(-0.165,2.02066721859313E-17,6.8));
#9841=CARTESIAN_POINT('',(-0.165,-2.02066721859313E-17,5.9));
#9842=CARTESIAN_POINT('Origin',(0.,0.,6.8));
#9843=CARTESIAN_POINT('Origin',(0.,0.,5.9));
#9844=CARTESIAN_POINT('Origin',(3.,0.,4.7));
#9845=CARTESIAN_POINT('',(2.75,-3.06161699786838E-17,4.8));
#9846=CARTESIAN_POINT('Origin',(3.,0.,4.8));
#9847=CARTESIAN_POINT('',(2.75,3.06161699786838E-17,5.2));
#9848=CARTESIAN_POINT('',(2.75,-3.06161699786838E-17,4.7));
#9849=CARTESIAN_POINT('Origin',(3.,0.,5.2));
#9850=CARTESIAN_POINT('Origin',(3.,0.,4.8));
#9851=CARTESIAN_POINT('',(3.,0.5,4.8));
#9852=CARTESIAN_POINT('',(3.,0.5,5.2));
#9853=CARTESIAN_POINT('',(3.,0.5,4.8));
#9854=CARTESIAN_POINT('',(3.,-0.5,5.2));
#9855=CARTESIAN_POINT('Origin',(3.,0.,5.2));
#9856=CARTESIAN_POINT('',(3.,-0.5,4.8));
#9857=CARTESIAN_POINT('',(3.,-0.5,4.8));
#9858=CARTESIAN_POINT('Origin',(3.,0.,4.8));
#9859=CARTESIAN_POINT('Origin',(0.,0.,4.8));
#9860=CARTESIAN_POINT('',(0.866025403784439,-0.5,4.8));
#9861=CARTESIAN_POINT('',(-2.5,-0.5,4.8));
#9862=CARTESIAN_POINT('',(-0.866025403784439,-0.5,4.8));
#9863=CARTESIAN_POINT('Origin',(0.,0.,4.8));
#9864=CARTESIAN_POINT('',(-2.5,-0.5,4.8));
#9865=CARTESIAN_POINT('',(-2.5,-0.5,4.8));
#9866=CARTESIAN_POINT('',(-2.5,0.5,4.8));
#9867=CARTESIAN_POINT('',(-2.5,0.5,4.8));
#9868=CARTESIAN_POINT('',(-0.866025403784439,0.5,4.8));
#9869=CARTESIAN_POINT('',(3.,0.5,4.8));
#9870=CARTESIAN_POINT('',(0.866025403784439,0.5,4.8));
#9871=CARTESIAN_POINT('Origin',(0.,0.,4.8));
#9872=CARTESIAN_POINT('',(3.,0.5,4.8));
#9873=CARTESIAN_POINT('',(-0.7,-8.57252759403147E-17,4.8));
#9874=CARTESIAN_POINT('Origin',(0.,0.,4.8));
#9875=CARTESIAN_POINT('Origin',(3.,0.5,4.8));
#9876=CARTESIAN_POINT('',(0.866025403784439,0.5,5.2));
#9877=CARTESIAN_POINT('',(0.866025403784439,0.5,4.8));
#9878=CARTESIAN_POINT('',(3.,0.5,5.2));
#9879=CARTESIAN_POINT('Origin',(-2.5,-0.5,4.8));
#9880=CARTESIAN_POINT('',(0.866025403784439,-0.5,5.2));
#9881=CARTESIAN_POINT('',(0.866025403784439,-0.5,4.8));
#9882=CARTESIAN_POINT('',(-2.5,-0.5,5.2));
#9883=CARTESIAN_POINT('Origin',(-2.5,-0.5,4.8));
#9884=CARTESIAN_POINT('',(-0.866025403784439,-0.5,5.2));
#9885=CARTESIAN_POINT('',(-0.866025403784439,-0.5,4.8));
#9886=CARTESIAN_POINT('',(-2.5,-0.5,5.2));
#9887=CARTESIAN_POINT('',(-2.5,-0.5,5.2));
#9888=CARTESIAN_POINT('',(-2.5,-0.5,4.8));
#9889=CARTESIAN_POINT('Origin',(3.,0.5,4.8));
#9890=CARTESIAN_POINT('',(-0.866025403784439,0.5,5.2));
#9891=CARTESIAN_POINT('',(-0.866025403784439,0.5,4.8));
#9892=CARTESIAN_POINT('',(-2.5,0.5,5.2));
#9893=CARTESIAN_POINT('',(-2.5,0.5,4.8));
#9894=CARTESIAN_POINT('',(3.,0.5,5.2));
#9895=CARTESIAN_POINT('Origin',(-2.5,0.5,4.8));
#9896=CARTESIAN_POINT('',(-2.5,0.5,5.2));
#9897=CARTESIAN_POINT('Origin',(0.,0.,5.2));
#9898=CARTESIAN_POINT('Origin',(0.,0.,5.2));
#9899=CARTESIAN_POINT('Origin',(0.,0.,5.2));
#9900=CARTESIAN_POINT('',(-0.5,-6.12323399573677E-17,5.2));
#9901=CARTESIAN_POINT('Origin',(0.,0.,5.2));
#9902=CARTESIAN_POINT('Origin',(0.,0.,4.8));
#9903=CARTESIAN_POINT('Origin',(0.,0.,4.8));
#9904=CARTESIAN_POINT('Origin',(0.,0.,2.95));
#9905=CARTESIAN_POINT('',(-0.7,-8.57252759403147E-17,2.95));
#9906=CARTESIAN_POINT('Origin',(0.,0.,2.95));
#9907=CARTESIAN_POINT('',(-0.5,6.12323399573677E-17,2.95));
#9908=CARTESIAN_POINT('Origin',(0.,0.,2.95));
#9909=CARTESIAN_POINT('Origin',(0.,0.,2.95));
#9910=CARTESIAN_POINT('',(-0.7,-8.57252759403147E-17,2.95));
#9911=CARTESIAN_POINT('Origin',(0.,0.,1.));
#9912=CARTESIAN_POINT('',(-0.5,-6.12323399573677E-17,1.));
#9913=CARTESIAN_POINT('',(-0.5,-6.12323399573677E-17,1.));
#9914=CARTESIAN_POINT('Origin',(0.,0.,1.));
#9915=CARTESIAN_POINT('Origin',(0.,0.,1.));
#9916=CARTESIAN_POINT('',(-0.5,-6.12323399573677E-17,6.8));
#9917=CARTESIAN_POINT('Origin',(0.,0.,6.8));
#9918=CARTESIAN_POINT('',(-0.5,-6.12323399573677E-17,1.));
#9919=CARTESIAN_POINT('Origin',(0.,0.,6.8));
#9920=CARTESIAN_POINT('Origin',(0.,0.,1.));
#9921=CARTESIAN_POINT('',(0.,0.,0.));
#9922=CARTESIAN_POINT('Origin',(0.,0.,1.8));
#9923=CARTESIAN_POINT('',(-0.505,-6.18446633569413E-17,2.05));
#9924=CARTESIAN_POINT('Origin',(0.,0.,2.05));
#9925=CARTESIAN_POINT('',(-0.505,-6.18446633569413E-17,1.8));
#9926=CARTESIAN_POINT('',(-0.505,-6.18446633569413E-17,1.8));
#9927=CARTESIAN_POINT('Origin',(0.,0.,1.8));
#9928=CARTESIAN_POINT('Origin',(0.,0.,1.8));
#9929=CARTESIAN_POINT('',(-0.7,-8.57252759403147E-17,2.05));
#9930=CARTESIAN_POINT('Origin',(0.,0.,2.05));
#9931=CARTESIAN_POINT('',(-0.7,-8.57252759403147E-17,1.8));
#9932=CARTESIAN_POINT('',(-0.7,-8.57252759403147E-17,1.8));
#9933=CARTESIAN_POINT('Origin',(0.,0.,1.8));
#9934=CARTESIAN_POINT('Origin',(0.,0.,2.05));
#9935=CARTESIAN_POINT('Origin',(0.,0.,1.8));
#9936=CARTESIAN_POINT('',(0.,0.,0.));
#9937=CARTESIAN_POINT('Origin',(0.,-0.49,1.4));
#9938=CARTESIAN_POINT('',(-0.122167917228706,-0.49,1.51090536506409));
#9939=CARTESIAN_POINT('',(-0.122167917228706,-0.49,1.28909463493591));
#9940=CARTESIAN_POINT('',(-0.122167917228706,-0.49,1.));
#9941=CARTESIAN_POINT('',(-0.165,-0.49,1.4));
#9942=CARTESIAN_POINT('Origin',(0.,-0.49,1.4));
#9943=CARTESIAN_POINT('Origin',(0.,-0.49,1.4));
#9944=CARTESIAN_POINT('Origin',(0.,-1.,1.4));
#9945=CARTESIAN_POINT('',(-0.165,-0.884745726183518,1.4));
#9946=CARTESIAN_POINT('Ctrl Pts',(-0.165,-0.884745726183518,1.4));
#9947=CARTESIAN_POINT('Ctrl Pts',(-0.165,-0.884745726183518,1.42076875940744));
#9948=CARTESIAN_POINT('Ctrl Pts',(-0.160839719007584,-0.885552759505264,
1.44288889507334));
#9949=CARTESIAN_POINT('Ctrl Pts',(-0.14398647021669,-0.888448648150043,
1.48352706263377));
#9950=CARTESIAN_POINT('Ctrl Pts',(-0.131295993814186,-0.890493604851638,
1.50204924397737));
#9951=CARTESIAN_POINT('Ctrl Pts',(-0.102049819008125,-0.89431723432394,
1.53129541878344));
#9952=CARTESIAN_POINT('Ctrl Pts',(-0.0835273920906823,-0.896347088899543,
1.54398634598358));
#9953=CARTESIAN_POINT('Ctrl Pts',(-0.0428883760934128,-0.899208271860583,
1.56083992183864));
#9954=CARTESIAN_POINT('Ctrl Pts',(-0.0207679427235068,-0.9,1.565));
#9955=CARTESIAN_POINT('Ctrl Pts',(0.0207679427235068,-0.9,1.565));
#9956=CARTESIAN_POINT('Ctrl Pts',(0.0428883760934127,-0.899208271860583,
1.56083992183864));
#9957=CARTESIAN_POINT('Ctrl Pts',(0.0835273920906823,-0.896347088899543,
1.54398634598358));
#9958=CARTESIAN_POINT('Ctrl Pts',(0.102049819008125,-0.89431723432394,1.53129541878344));
#9959=CARTESIAN_POINT('Ctrl Pts',(0.131295993814186,-0.890493604851638,
1.50204924397737));
#9960=CARTESIAN_POINT('Ctrl Pts',(0.14398647021669,-0.888448648150043,1.48352706263377));
#9961=CARTESIAN_POINT('Ctrl Pts',(0.160839719007584,-0.885552759505264,
1.44288889507334));
#9962=CARTESIAN_POINT('Ctrl Pts',(0.165,-0.884745726183518,1.42076875940744));
#9963=CARTESIAN_POINT('Ctrl Pts',(0.165,-0.884745726183518,1.37923124059256));
#9964=CARTESIAN_POINT('Ctrl Pts',(0.160839719007584,-0.885552759505264,
1.35711110492666));
#9965=CARTESIAN_POINT('Ctrl Pts',(0.14398647021669,-0.888448648150043,1.31647293736623));
#9966=CARTESIAN_POINT('Ctrl Pts',(0.131295993814186,-0.890493604851638,
1.29795075602263));
#9967=CARTESIAN_POINT('Ctrl Pts',(0.102049819008125,-0.89431723432394,1.26870458121656));
#9968=CARTESIAN_POINT('Ctrl Pts',(0.0835273920906823,-0.896347088899543,
1.25601365401642));
#9969=CARTESIAN_POINT('Ctrl Pts',(0.0428883760934127,-0.899208271860583,
1.23916007816136));
#9970=CARTESIAN_POINT('Ctrl Pts',(0.0207679427235068,-0.9,1.235));
#9971=CARTESIAN_POINT('Ctrl Pts',(-0.0207679427235067,-0.9,1.235));
#9972=CARTESIAN_POINT('Ctrl Pts',(-0.0428883760934127,-0.899208271860583,
1.23916007816136));
#9973=CARTESIAN_POINT('Ctrl Pts',(-0.0835273920906822,-0.896347088899543,
1.25601365401642));
#9974=CARTESIAN_POINT('Ctrl Pts',(-0.102049819008125,-0.89431723432394,
1.26870458121656));
#9975=CARTESIAN_POINT('Ctrl Pts',(-0.131295993814186,-0.890493604851638,
1.29795075602263));
#9976=CARTESIAN_POINT('Ctrl Pts',(-0.14398647021669,-0.888448648150043,
1.31647293736623));
#9977=CARTESIAN_POINT('Ctrl Pts',(-0.160839719007584,-0.885552759505264,
1.35711110492666));
#9978=CARTESIAN_POINT('Ctrl Pts',(-0.165,-0.884745726183518,1.37923124059256));
#9979=CARTESIAN_POINT('Ctrl Pts',(-0.165,-0.884745726183518,1.4));
#9980=CARTESIAN_POINT('',(-0.165,-1.,1.4));
#9981=CARTESIAN_POINT('',(0.122167917228706,-0.49,1.51090536506409));
#9982=CARTESIAN_POINT('Ctrl Pts',(0.122167917228706,-0.49,1.51090536506409));
#9983=CARTESIAN_POINT('Ctrl Pts',(0.120368913626296,-0.490448531679987,
1.51288705930464));
#9984=CARTESIAN_POINT('Ctrl Pts',(0.118534896565231,-0.490895245371684,
1.51481034122633));
#9985=CARTESIAN_POINT('Ctrl Pts',(0.102111993019358,-0.494795015531646,
1.5312332447722));
#9986=CARTESIAN_POINT('Ctrl Pts',(0.0836597150224318,-0.498442514607594,
1.54390845611142));
#9987=CARTESIAN_POINT('Ctrl Pts',(0.0430495960471595,-0.50357781976106,
1.56079590960766));
#9988=CARTESIAN_POINT('Ctrl Pts',(0.020880094330741,-0.505,1.565));
#9989=CARTESIAN_POINT('Ctrl Pts',(-0.020880094330741,-0.505,1.565));
#9990=CARTESIAN_POINT('Ctrl Pts',(-0.0430495960471594,-0.50357781976106,
1.56079590960766));
#9991=CARTESIAN_POINT('Ctrl Pts',(-0.0836597150224317,-0.498442514607594,
1.54390845611142));
#9992=CARTESIAN_POINT('Ctrl Pts',(-0.102111993019358,-0.494795015531646,
1.5312332447722));
#9993=CARTESIAN_POINT('Ctrl Pts',(-0.118534896565231,-0.490895245371684,
1.51481034122633));
#9994=CARTESIAN_POINT('Ctrl Pts',(-0.120368913626296,-0.490448531679987,
1.51288705930464));
#9995=CARTESIAN_POINT('Ctrl Pts',(-0.122167917228706,-0.49,1.51090536506409));
#9996=CARTESIAN_POINT('',(0.122167917228706,-0.49,1.28909463493591));
#9997=CARTESIAN_POINT('Origin',(0.,-0.49,1.4));
#9998=CARTESIAN_POINT('Ctrl Pts',(-0.122167917228706,-0.49,1.28909463493591));
#9999=CARTESIAN_POINT('Ctrl Pts',(-0.120368913626296,-0.490448531679987,
1.28711294069536));
#10000=CARTESIAN_POINT('Ctrl Pts',(-0.118534896565231,-0.490895245371684,
1.28518965877367));
#10001=CARTESIAN_POINT('Ctrl Pts',(-0.102111993019358,-0.494795015531646,
1.2687667552278));
#10002=CARTESIAN_POINT('Ctrl Pts',(-0.0836597150224318,-0.498442514607594,
1.25609154388858));
#10003=CARTESIAN_POINT('Ctrl Pts',(-0.0430495960471595,-0.50357781976106,
1.23920409039234));
#10004=CARTESIAN_POINT('Ctrl Pts',(-0.020880094330741,-0.505,1.235));
#10005=CARTESIAN_POINT('Ctrl Pts',(0.020880094330741,-0.505,1.235));
#10006=CARTESIAN_POINT('Ctrl Pts',(0.0430495960471595,-0.50357781976106,
1.23920409039234));
#10007=CARTESIAN_POINT('Ctrl Pts',(0.0836597150224318,-0.498442514607594,
1.25609154388858));
#10008=CARTESIAN_POINT('Ctrl Pts',(0.102111993019358,-0.494795015531646,
1.2687667552278));
#10009=CARTESIAN_POINT('Ctrl Pts',(0.118534896565231,-0.490895245371684,
1.28518965877367));
#10010=CARTESIAN_POINT('Ctrl Pts',(0.120368913626296,-0.490448531679987,
1.28711294069536));
#10011=CARTESIAN_POINT('Ctrl Pts',(0.122167917228706,-0.49,1.28909463493591));
#10012=CARTESIAN_POINT('Origin',(0.,-0.49,1.4));
#10013=CARTESIAN_POINT('',(0.122167917228706,-0.49,1.));
#10014=CARTESIAN_POINT('Origin',(-0.49,0.,1.4));
#10015=CARTESIAN_POINT('',(-0.49,0.122167917228706,1.51090536506409));
#10016=CARTESIAN_POINT('',(-0.49,0.122167917228706,1.28909463493591));
#10017=CARTESIAN_POINT('',(-0.49,0.122167917228706,1.));
#10018=CARTESIAN_POINT('Origin',(-0.49,0.,1.4));
#10019=CARTESIAN_POINT('Origin',(-1.,0.,1.4));
#10020=CARTESIAN_POINT('',(-0.884745726183518,0.165,1.4));
#10021=CARTESIAN_POINT('',(-0.9,-2.02066721859313E-17,1.565));
#10022=CARTESIAN_POINT('Ctrl Pts',(-0.884745726183518,0.165,1.4));
#10023=CARTESIAN_POINT('Ctrl Pts',(-0.884745726183518,0.165,1.42076875940744));
#10024=CARTESIAN_POINT('Ctrl Pts',(-0.885552759505264,0.160839719007584,
1.44288889507334));
#10025=CARTESIAN_POINT('Ctrl Pts',(-0.888448648150043,0.14398647021669,
1.48352706263377));
#10026=CARTESIAN_POINT('Ctrl Pts',(-0.890493604851638,0.131295993814186,
1.50204924397737));
#10027=CARTESIAN_POINT('Ctrl Pts',(-0.89431723432394,0.102049819008125,
1.53129541878344));
#10028=CARTESIAN_POINT('Ctrl Pts',(-0.896347088899543,0.0835273920906824,
1.54398634598358));
#10029=CARTESIAN_POINT('Ctrl Pts',(-0.899208271860583,0.0428883760934128,
1.56083992183864));
#10030=CARTESIAN_POINT('Ctrl Pts',(-0.9,0.0207679427235068,1.565));
#10031=CARTESIAN_POINT('Ctrl Pts',(-0.9,2.77555756156289E-17,1.565));
#10032=CARTESIAN_POINT('',(-0.9,-8.63341285292134E-17,1.235));
#10033=CARTESIAN_POINT('Ctrl Pts',(-0.9,-6.24500451351651E-17,1.235));
#10034=CARTESIAN_POINT('Ctrl Pts',(-0.9,0.0207679427235068,1.235));
#10035=CARTESIAN_POINT('Ctrl Pts',(-0.899208271860583,0.0428883760934128,
1.23916007816136));
#10036=CARTESIAN_POINT('Ctrl Pts',(-0.896347088899543,0.0835273920906824,
1.25601365401642));
#10037=CARTESIAN_POINT('Ctrl Pts',(-0.89431723432394,0.102049819008125,
1.26870458121656));
#10038=CARTESIAN_POINT('Ctrl Pts',(-0.890493604851638,0.131295993814186,
1.29795075602263));
#10039=CARTESIAN_POINT('Ctrl Pts',(-0.888448648150043,0.143986470216691,
1.31647293736623));
#10040=CARTESIAN_POINT('Ctrl Pts',(-0.885552759505264,0.160839719007584,
1.35711110492666));
#10041=CARTESIAN_POINT('Ctrl Pts',(-0.884745726183518,0.165,1.37923124059256));
#10042=CARTESIAN_POINT('Ctrl Pts',(-0.884745726183518,0.165,1.4));
#10043=CARTESIAN_POINT('Ctrl Pts',(-0.9,4.16333634234434E-17,1.565));
#10044=CARTESIAN_POINT('Ctrl Pts',(-0.9,-0.0207679427235068,1.565));
#10045=CARTESIAN_POINT('Ctrl Pts',(-0.899208271860583,-0.0428883760934127,
1.56083992183864));
#10046=CARTESIAN_POINT('Ctrl Pts',(-0.896347088899543,-0.0835273920906824,
1.54398634598358));
#10047=CARTESIAN_POINT('Ctrl Pts',(-0.89431723432394,-0.102049819008125,
1.53129541878344));
#10048=CARTESIAN_POINT('Ctrl Pts',(-0.890493604851638,-0.131295993814186,
1.50204924397737));
#10049=CARTESIAN_POINT('Ctrl Pts',(-0.888448648150043,-0.143986470216691,
1.48352706263377));
#10050=CARTESIAN_POINT('Ctrl Pts',(-0.885552759505264,-0.160839719007584,
1.44288889507334));
#10051=CARTESIAN_POINT('Ctrl Pts',(-0.884745726183518,-0.165,1.42076875940744));
#10052=CARTESIAN_POINT('Ctrl Pts',(-0.884745726183518,-0.165,1.37923124059256));
#10053=CARTESIAN_POINT('Ctrl Pts',(-0.885552759505264,-0.160839719007584,
1.35711110492666));
#10054=CARTESIAN_POINT('Ctrl Pts',(-0.888448648150043,-0.14398647021669,
1.31647293736623));
#10055=CARTESIAN_POINT('Ctrl Pts',(-0.890493604851638,-0.131295993814186,
1.29795075602263));
#10056=CARTESIAN_POINT('Ctrl Pts',(-0.89431723432394,-0.102049819008125,
1.26870458121656));
#10057=CARTESIAN_POINT('Ctrl Pts',(-0.896347088899543,-0.0835273920906825,
1.25601365401642));
#10058=CARTESIAN_POINT('Ctrl Pts',(-0.899208271860583,-0.0428883760934129,
1.23916007816136));
#10059=CARTESIAN_POINT('Ctrl Pts',(-0.9,-0.0207679427235069,1.235));
#10060=CARTESIAN_POINT('Ctrl Pts',(-0.9,-4.85722573273506E-17,1.235));
#10061=CARTESIAN_POINT('',(-0.505,-2.74505708527337E-17,1.565));
#10062=CARTESIAN_POINT('',(-1.,-2.02066721859313E-17,1.565));
#10063=CARTESIAN_POINT('',(-0.49,-0.122167917228706,1.51090536506409));
#10064=CARTESIAN_POINT('Ctrl Pts',(-0.49,-0.122167917228706,1.51090536506409));
#10065=CARTESIAN_POINT('Ctrl Pts',(-0.490448531679987,-0.120368913626296,
1.51288705930464));
#10066=CARTESIAN_POINT('Ctrl Pts',(-0.490895245371684,-0.118534896565231,
1.51481034122633));
#10067=CARTESIAN_POINT('Ctrl Pts',(-0.494795015531646,-0.102111993019358,
1.5312332447722));
#10068=CARTESIAN_POINT('Ctrl Pts',(-0.498442514607594,-0.0836597150224318,
1.54390845611142));
#10069=CARTESIAN_POINT('Ctrl Pts',(-0.50357781976106,-0.0430495960471595,
1.56079590960766));
#10070=CARTESIAN_POINT('Ctrl Pts',(-0.505,-0.020880094330741,1.565));
#10071=CARTESIAN_POINT('Ctrl Pts',(-0.505,0.,1.565));
#10072=CARTESIAN_POINT('',(-0.49,-0.122167917228706,1.28909463493591));
#10073=CARTESIAN_POINT('Origin',(-0.49,0.,1.4));
#10074=CARTESIAN_POINT('',(-0.505,-2.05139908226098E-17,1.235));
#10075=CARTESIAN_POINT('Ctrl Pts',(-0.505,2.77555756156289E-17,1.235));
#10076=CARTESIAN_POINT('Ctrl Pts',(-0.505,-0.020880094330741,1.235));
#10077=CARTESIAN_POINT('Ctrl Pts',(-0.50357781976106,-0.0430495960471594,
1.23920409039234));
#10078=CARTESIAN_POINT('Ctrl Pts',(-0.498442514607595,-0.0836597150224317,
1.25609154388858));
#10079=CARTESIAN_POINT('Ctrl Pts',(-0.494795015531646,-0.102111993019358,
1.2687667552278));
#10080=CARTESIAN_POINT('Ctrl Pts',(-0.490895245371684,-0.118534896565231,
1.28518965877367));
#10081=CARTESIAN_POINT('Ctrl Pts',(-0.490448531679987,-0.120368913626296,
1.28711294069536));
#10082=CARTESIAN_POINT('Ctrl Pts',(-0.49,-0.122167917228706,1.28909463493591));
#10083=CARTESIAN_POINT('Ctrl Pts',(-0.49,0.122167917228706,1.28909463493591));
#10084=CARTESIAN_POINT('Ctrl Pts',(-0.490448531679987,0.120368913626296,
1.28711294069536));
#10085=CARTESIAN_POINT('Ctrl Pts',(-0.490895245371684,0.118534896565231,
1.28518965877367));
#10086=CARTESIAN_POINT('Ctrl Pts',(-0.494795015531646,0.102111993019358,
1.2687667552278));
#10087=CARTESIAN_POINT('Ctrl Pts',(-0.498442514607594,0.0836597150224318,
1.25609154388858));
#10088=CARTESIAN_POINT('Ctrl Pts',(-0.50357781976106,0.0430495960471595,
1.23920409039234));
#10089=CARTESIAN_POINT('Ctrl Pts',(-0.505,0.020880094330741,1.235));
#10090=CARTESIAN_POINT('Ctrl Pts',(-0.505,-6.93889390390723E-18,1.235));
#10091=CARTESIAN_POINT('Ctrl Pts',(-0.505,-2.77555756156289E-17,1.565));
#10092=CARTESIAN_POINT('Ctrl Pts',(-0.505,0.020880094330741,1.565));
#10093=CARTESIAN_POINT('Ctrl Pts',(-0.50357781976106,0.0430495960471595,
1.56079590960766));
#10094=CARTESIAN_POINT('Ctrl Pts',(-0.498442514607594,0.0836597150224318,
1.54390845611142));
#10095=CARTESIAN_POINT('Ctrl Pts',(-0.494795015531646,0.102111993019358,
1.5312332447722));
#10096=CARTESIAN_POINT('Ctrl Pts',(-0.490895245371684,0.118534896565231,
1.51481034122633));
#10097=CARTESIAN_POINT('Ctrl Pts',(-0.490448531679987,0.120368913626296,
1.51288705930464));
#10098=CARTESIAN_POINT('Ctrl Pts',(-0.49,0.122167917228706,1.51090536506409));
#10099=CARTESIAN_POINT('Origin',(-0.49,0.,1.4));
#10100=CARTESIAN_POINT('',(-0.49,-0.122167917228706,1.));
#10101=CARTESIAN_POINT('Origin',(0.,0.,1.));
#10102=CARTESIAN_POINT('',(-0.505,-6.18446633569413E-17,1.8));
#10103=CARTESIAN_POINT('Origin',(0.,0.,1.8));
#10104=CARTESIAN_POINT('',(-0.505,-6.18446633569413E-17,1.));
#10105=CARTESIAN_POINT('',(-0.505,-6.18446633569413E-17,1.));
#10106=CARTESIAN_POINT('',(-0.505,-6.18446633569413E-17,1.));
#10107=CARTESIAN_POINT('Origin',(0.,0.,1.));
#10108=CARTESIAN_POINT('Origin',(0.,0.,1.));
#10109=CARTESIAN_POINT('',(-0.9,-1.10218211923262E-16,1.8));
#10110=CARTESIAN_POINT('Origin',(0.,0.,1.8));
#10111=CARTESIAN_POINT('',(-0.9,-1.10218211923262E-16,1.));
#10112=CARTESIAN_POINT('',(-0.9,-1.10218211923262E-16,1.));
#10113=CARTESIAN_POINT('',(-0.9,-1.10218211923262E-16,1.));
#10114=CARTESIAN_POINT('Origin',(0.,0.,1.));
#10115=CARTESIAN_POINT('Origin',(0.,0.,1.8));
#10116=CARTESIAN_POINT('Origin',(0.,0.,1.));
#10117=CARTESIAN_POINT('',(0.,0.,0.));
#10118=CARTESIAN_POINT('Origin',(3.,0.,5.6));
#10119=CARTESIAN_POINT('',(2.5,-6.12323399573677E-17,5.6));
#10120=CARTESIAN_POINT('Origin',(3.,0.,5.6));
#10121=CARTESIAN_POINT('',(2.7,-3.67394039744206E-17,5.6));
#10122=CARTESIAN_POINT('Origin',(3.,0.,5.6));
#10123=CARTESIAN_POINT('Origin',(3.,0.,5.2));
#10124=CARTESIAN_POINT('',(2.5,-6.12323399573677E-17,5.2));
#10125=CARTESIAN_POINT('Origin',(3.,0.,5.2));
#10126=CARTESIAN_POINT('',(2.7,3.67394039744206E-17,5.2));
#10127=CARTESIAN_POINT('Origin',(3.,0.,5.2));
#10128=CARTESIAN_POINT('Origin',(3.,0.,5.2));
#10129=CARTESIAN_POINT('',(2.5,-6.12323399573677E-17,5.2));
#10130=CARTESIAN_POINT('Origin',(3.,0.,4.8));
#10131=CARTESIAN_POINT('',(2.7,-3.67394039744206E-17,4.8));
#10132=CARTESIAN_POINT('',(2.7,-3.67394039744206E-17,4.8));
#10133=CARTESIAN_POINT('Origin',(3.,0.,4.8));
#10134=CARTESIAN_POINT('Origin',(3.,0.,4.8));
#10135=CARTESIAN_POINT('',(2.7,-3.67394039744206E-17,7.));
#10136=CARTESIAN_POINT('Origin',(3.,0.,7.));
#10137=CARTESIAN_POINT('',(2.7,-3.67394039744206E-17,4.8));
#10138=CARTESIAN_POINT('Origin',(3.,0.,7.));
#10139=CARTESIAN_POINT('Origin',(3.,0.,4.8));
#10140=CARTESIAN_POINT('',(0.,0.,0.));
#10141=CARTESIAN_POINT('Origin',(0.,0.,5.9));
#10142=CARTESIAN_POINT('',(-0.5,-6.12323399573677E-17,6.));
#10143=CARTESIAN_POINT('Origin',(0.,0.,6.));
#10144=CARTESIAN_POINT('',(-0.5,6.12323399573677E-17,6.8));
#10145=CARTESIAN_POINT('',(-0.5,-6.12323399573677E-17,5.9));
#10146=CARTESIAN_POINT('Origin',(0.,0.,6.8));
#10147=CARTESIAN_POINT('Origin',(0.,0.,6.));
#10148=CARTESIAN_POINT('',(0.,0.6,6.8));
#10149=CARTESIAN_POINT('',(0.,0.6,6.));
#10150=CARTESIAN_POINT('',(0.,0.6,6.));
#10151=CARTESIAN_POINT('',(0.,-0.6,6.8));
#10152=CARTESIAN_POINT('Origin',(0.,0.,6.8));
#10153=CARTESIAN_POINT('',(0.,-0.6,6.));
#10154=CARTESIAN_POINT('',(0.,-0.6,6.));
#10155=CARTESIAN_POINT('Origin',(0.,0.,6.));
#10156=CARTESIAN_POINT('Origin',(0.,0.,6.));
#10157=CARTESIAN_POINT('',(0.,-1.8,6.));
#10158=CARTESIAN_POINT('',(0.,0.95,6.));
#10159=CARTESIAN_POINT('',(0.,1.8,6.));
#10160=CARTESIAN_POINT('Origin',(0.,0.,6.));
#10161=CARTESIAN_POINT('',(0.,0.95,6.));
#10162=CARTESIAN_POINT('Origin',(0.,1.9,5.9));
#10163=CARTESIAN_POINT('',(0.,-1.8,6.8));
#10164=CARTESIAN_POINT('',(0.,0.95,6.8));
#10165=CARTESIAN_POINT('',(0.,-1.8,6.));
#10166=CARTESIAN_POINT('Origin',(0.,1.9,5.9));
#10167=CARTESIAN_POINT('',(0.,1.8,6.8));
#10168=CARTESIAN_POINT('',(0.,1.8,6.));
#10169=CARTESIAN_POINT('',(0.,0.95,6.8));
#10170=CARTESIAN_POINT('Origin',(0.,0.,6.));
#10171=CARTESIAN_POINT('Origin',(0.,0.,6.8));
#10172=CARTESIAN_POINT('Origin',(0.,0.,6.8));
#10173=CARTESIAN_POINT('',(0.,0.,0.));
#10174=CARTESIAN_POINT('Origin',(0.,0.,5.2));
#10175=CARTESIAN_POINT('',(-0.505,-6.18446633569413E-17,6.));
#10176=CARTESIAN_POINT('Origin',(0.,0.,6.));
#10177=CARTESIAN_POINT('',(-0.505,-6.18446633569413E-17,5.2));
#10178=CARTESIAN_POINT('',(-0.505,-6.18446633569413E-17,5.2));
#10179=CARTESIAN_POINT('Origin',(0.,0.,5.2));
#10180=CARTESIAN_POINT('Origin',(0.,0.,5.2));
#10181=CARTESIAN_POINT('',(-0.7,-8.57252759403147E-17,6.));
#10182=CARTESIAN_POINT('Origin',(0.,0.,6.));
#10183=CARTESIAN_POINT('',(-0.7,-8.57252759403147E-17,5.2));
#10184=CARTESIAN_POINT('',(-0.7,-8.57252759403147E-17,5.2));
#10185=CARTESIAN_POINT('Origin',(0.,0.,5.2));
#10186=CARTESIAN_POINT('Origin',(0.,0.,6.));
#10187=CARTESIAN_POINT('Origin',(0.,0.,5.2));
#10188=CARTESIAN_POINT('',(0.,0.,0.));
#10189=CARTESIAN_POINT('Origin',(0.,0.,6.8));
#10190=CARTESIAN_POINT('',(-0.225,-2.75545529808154E-17,7.));
#10191=CARTESIAN_POINT('Origin',(0.,0.,7.));
#10192=CARTESIAN_POINT('',(-0.225,-2.75545529808154E-17,6.8));
#10193=CARTESIAN_POINT('',(-0.225,-2.75545529808154E-17,6.8));
#10194=CARTESIAN_POINT('Origin',(0.,0.,6.8));
#10195=CARTESIAN_POINT('Origin',(0.,0.,6.8));
#10196=CARTESIAN_POINT('',(-0.7,-8.57252759403147E-17,7.));
#10197=CARTESIAN_POINT('Origin',(0.,0.,7.));
#10198=CARTESIAN_POINT('',(-0.7,-8.57252759403147E-17,6.8));
#10199=CARTESIAN_POINT('',(-0.7,-8.57252759403147E-17,6.8));
#10200=CARTESIAN_POINT('Origin',(0.,0.,6.8));
#10201=CARTESIAN_POINT('Origin',(0.,0.,7.));
#10202=CARTESIAN_POINT('Origin',(0.,0.,6.8));
#10203=CARTESIAN_POINT('',(0.,0.,0.));
#10204=CARTESIAN_POINT('Origin',(0.,0.,7.));
#10205=CARTESIAN_POINT('',(-0.4,-4.89858719658941E-17,8.5));
#10206=CARTESIAN_POINT('Origin',(0.,0.,8.5));
#10207=CARTESIAN_POINT('',(-0.4,-4.89858719658941E-17,7.));
#10208=CARTESIAN_POINT('',(-0.4,-4.89858719658941E-17,7.));
#10209=CARTESIAN_POINT('Origin',(0.,0.,7.));
#10210=CARTESIAN_POINT('Origin',(0.,0.,7.));
#10211=CARTESIAN_POINT('',(-1.4,-1.71450551880629E-16,8.5));
#10212=CARTESIAN_POINT('Origin',(0.,0.,8.5));
#10213=CARTESIAN_POINT('',(-1.4,-1.71450551880629E-16,7.));
#10214=CARTESIAN_POINT('',(-1.4,-1.71450551880629E-16,7.));
#10215=CARTESIAN_POINT('Origin',(0.,0.,7.));
#10216=CARTESIAN_POINT('Origin',(0.,0.,8.5));
#10217=CARTESIAN_POINT('Origin',(0.,0.,7.));
#10218=CARTESIAN_POINT('',(0.,0.,0.));
#10219=CARTESIAN_POINT('Origin',(0.0866025403784439,-0.4,-0.15));
#10220=CARTESIAN_POINT('',(0.173205080756888,-0.4,0.));
#10221=CARTESIAN_POINT('',(0.0866025403784439,-0.4,-0.15));
#10222=CARTESIAN_POINT('',(0.173205080756888,-0.4,0.));
#10223=CARTESIAN_POINT('',(0.0866025403784439,-0.64,-0.15));
#10224=CARTESIAN_POINT('',(0.0866025403784439,-0.4,-0.15));
#10225=CARTESIAN_POINT('',(0.173205080756888,-0.64,0.));
#10226=CARTESIAN_POINT('',(0.173205080756888,-0.64,0.));
#10227=CARTESIAN_POINT('',(0.173205080756888,-0.4,0.));
#10228=CARTESIAN_POINT('Origin',(-0.0866025403784438,-0.4,-0.15));
#10229=CARTESIAN_POINT('',(-0.0866025403784438,-0.4,-0.15));
#10230=CARTESIAN_POINT('',(0.0866025403784439,-0.4,-0.15));
#10231=CARTESIAN_POINT('',(-0.0866025403784438,-0.64,-0.15));
#10232=CARTESIAN_POINT('',(-0.0866025403784438,-0.4,-0.15));
#10233=CARTESIAN_POINT('',(0.0866025403784439,-0.64,-0.15));
#10234=CARTESIAN_POINT('Origin',(-0.173205080756888,-0.4,-2.77555756156289E-17));
#10235=CARTESIAN_POINT('',(-0.173205080756888,-0.4,-2.12115047744981E-17));
#10236=CARTESIAN_POINT('',(-0.0866025403784438,-0.4,-0.15));
#10237=CARTESIAN_POINT('',(-0.173205080756888,-0.64,-2.77555756156289E-17));
#10238=CARTESIAN_POINT('',(-0.173205080756888,-0.4,-2.12115047744981E-17));
#10239=CARTESIAN_POINT('',(-0.0866025403784438,-0.64,-0.15));
#10240=CARTESIAN_POINT('Origin',(-0.0866025403784439,-0.4,0.15));
#10241=CARTESIAN_POINT('',(-0.0866025403784439,-0.4,0.15));
#10242=CARTESIAN_POINT('',(-0.173205080756888,-0.4,-2.12115047744981E-17));
#10243=CARTESIAN_POINT('',(-0.0866025403784439,-0.64,0.15));
#10244=CARTESIAN_POINT('',(-0.0866025403784439,-0.4,0.15));
#10245=CARTESIAN_POINT('',(-0.173205080756888,-0.64,-2.12115047744981E-17));
#10246=CARTESIAN_POINT('Origin',(0.0866025403784439,-0.4,0.15));
#10247=CARTESIAN_POINT('',(0.0866025403784439,-0.4,0.15));
#10248=CARTESIAN_POINT('',(-0.0866025403784439,-0.4,0.15));
#10249=CARTESIAN_POINT('',(0.0866025403784439,-0.64,0.15));
#10250=CARTESIAN_POINT('',(0.0866025403784439,-0.4,0.15));
#10251=CARTESIAN_POINT('',(-0.0866025403784439,-0.64,0.15));
#10252=CARTESIAN_POINT('Origin',(0.173205080756888,-0.4,0.));
#10253=CARTESIAN_POINT('',(0.0866025403784439,-0.4,0.15));
#10254=CARTESIAN_POINT('',(0.0866025403784439,-0.64,0.15));
#10255=CARTESIAN_POINT('Origin',(0.,-0.4,-2.77555756156289E-17));
#10256=CARTESIAN_POINT('Origin',(0.,-0.64,-2.77555756156289E-17));
#10257=CARTESIAN_POINT('Origin',(0.,-1.,0.));
#10258=CARTESIAN_POINT('',(-0.1954,-1.,2.39295984553393E-17));
#10259=CARTESIAN_POINT('Origin',(0.,-1.,0.));
#10260=CARTESIAN_POINT('Origin',(0.3,0.4,0.));
#10261=CARTESIAN_POINT('',(-0.3,0.4,-3.67394039744206E-17));
#10262=CARTESIAN_POINT('Origin',(0.,0.4,0.));
#10263=CARTESIAN_POINT('Origin',(0.,0.375,0.));
#10264=CARTESIAN_POINT('',(-0.35,0.35,-4.28626379701573E-17));
#10265=CARTESIAN_POINT('Origin',(0.,0.35,0.));
#10266=CARTESIAN_POINT('',(-0.325,0.375,-3.9801020972289E-17));
#10267=CARTESIAN_POINT('Origin',(0.,0.19,0.));
#10268=CARTESIAN_POINT('',(-0.35,0.03,-4.28626379701574E-17));
#10269=CARTESIAN_POINT('Origin',(0.,0.03,0.));
#10270=CARTESIAN_POINT('',(-0.35,0.19,-4.28626379701574E-17));
#10271=CARTESIAN_POINT('Origin',(0.,0.0149999999999999,0.));
#10272=CARTESIAN_POINT('',(-0.32,-3.29597460435593E-17,-3.91886975727153E-17));
#10273=CARTESIAN_POINT('Origin',(0.,0.,0.));
#10274=CARTESIAN_POINT('',(-0.335,0.0149999999999999,-4.10256677714363E-17));
#10275=CARTESIAN_POINT('Origin',(0.22,0.,0.));
#10276=CARTESIAN_POINT('',(-0.22,-6.93889390390723E-18,-2.69422295812418E-17));
#10277=CARTESIAN_POINT('Origin',(0.,0.,0.));
#10278=CARTESIAN_POINT('Origin',(0.,-0.02,0.));
#10279=CARTESIAN_POINT('',(-0.1954,-0.0492,2.39295984553393E-17));
#10280=CARTESIAN_POINT('Origin',(0.,-0.0492,0.));
#10281=CARTESIAN_POINT('',(-0.21,-0.02,-2.57175827820944E-17));
#10282=CARTESIAN_POINT('Origin',(0.,-0.8,0.));
#10283=CARTESIAN_POINT('',(-0.1954,-0.8,-2.39295984553393E-17));
#10284=CARTESIAN_POINT('',(0.,0.,0.));
#10285=CARTESIAN_POINT('',(0.,0.,0.));
#10286=CARTESIAN_POINT('',(0.,0.,0.));
#10287=CARTESIAN_POINT('',(0.,0.,0.));
#10288=CARTESIAN_POINT('',(0.,0.,0.));
#10289=CARTESIAN_POINT('',(0.,0.,0.));
#10290=CARTESIAN_POINT('',(-1.7,-1.7,2.2));
#10291=CARTESIAN_POINT('',(-1.7,1.7,2.2));
#10292=CARTESIAN_POINT('',(5.94264068711928,-1.7,2.2));
#10293=CARTESIAN_POINT('',(5.94264068711928,1.7,2.2));
#10294=CARTESIAN_POINT('',(0.,0.,2.5));
#10295=CARTESIAN_POINT('',(1.72,0.,4.));
#10296=CARTESIAN_POINT('',(0.,1.72,4.));
#10297=CARTESIAN_POINT('',(-1.72,2.10639249453345E-16,4.));
#10298=CARTESIAN_POINT('',(-2.22044604925031E-16,-1.72,4.));
#10299=CARTESIAN_POINT('',(4.24264068711929,0.,2.5));
#10300=CARTESIAN_POINT('',(5.96264068711929,0.,4.));
#10301=CARTESIAN_POINT('',(4.24264068711929,1.72,4.));
#10302=CARTESIAN_POINT('',(2.52264068711929,2.10639249453345E-16,4.));
#10303=CARTESIAN_POINT('',(4.24264068711929,-1.72,4.));
#10304=CARTESIAN_POINT('',(0.,0.,0.));
#10305=CARTESIAN_POINT('',(0.,0.,0.));
#10306=CARTESIAN_POINT('Origin',(2.9698484809835,-1.27279220613579,5.9));
#10307=CARTESIAN_POINT('',(2.8048484809835,-1.27279220613579,6.));
#10308=CARTESIAN_POINT('Origin',(2.9698484809835,-1.27279220613579,6.));
#10309=CARTESIAN_POINT('',(2.8048484809835,-1.27279220613579,6.8));
#10310=CARTESIAN_POINT('',(2.8048484809835,-1.27279220613579,5.9));
#10311=CARTESIAN_POINT('Origin',(2.9698484809835,-1.27279220613579,6.8));
#10312=CARTESIAN_POINT('Origin',(2.9698484809835,1.27279220613579,5.9));
#10313=CARTESIAN_POINT('',(2.8048484809835,1.27279220613579,6.));
#10314=CARTESIAN_POINT('Origin',(2.9698484809835,1.27279220613579,6.));
#10315=CARTESIAN_POINT('',(2.8048484809835,1.27279220613579,6.8));
#10316=CARTESIAN_POINT('',(2.8048484809835,1.27279220613579,5.9));
#10317=CARTESIAN_POINT('Origin',(2.9698484809835,1.27279220613579,6.8));
#10318=CARTESIAN_POINT('Origin',(5.51543289325507,1.27279220613579,5.9));
#10319=CARTESIAN_POINT('',(5.35043289325507,1.27279220613579,6.));
#10320=CARTESIAN_POINT('Origin',(5.51543289325507,1.27279220613579,6.));
#10321=CARTESIAN_POINT('',(5.35043289325507,1.27279220613579,6.8));
#10322=CARTESIAN_POINT('',(5.35043289325507,1.27279220613579,5.9));
#10323=CARTESIAN_POINT('Origin',(5.51543289325507,1.27279220613579,6.8));
#10324=CARTESIAN_POINT('Origin',(5.51543289325507,-1.27279220613579,5.9));
#10325=CARTESIAN_POINT('',(5.35043289325507,-1.27279220613579,6.));
#10326=CARTESIAN_POINT('Origin',(5.51543289325507,-1.27279220613579,6.));
#10327=CARTESIAN_POINT('',(5.35043289325507,-1.27279220613579,6.8));
#10328=CARTESIAN_POINT('',(5.35043289325507,-1.27279220613579,5.9));
#10329=CARTESIAN_POINT('Origin',(5.51543289325507,-1.27279220613579,6.8));
#10330=CARTESIAN_POINT('Origin',(1.24264068711928,-3.,5.9));
#10331=CARTESIAN_POINT('',(3.04549806673909,-2.75079071295314,6.));
#10332=CARTESIAN_POINT('',(1.49184997416615,-1.19714262038019,6.));
#10333=CARTESIAN_POINT('Origin',(1.24264068711928,-3.,6.));
#10334=CARTESIAN_POINT('',(3.04549806673909,-2.75079071295314,6.8));
#10335=CARTESIAN_POINT('',(3.04549806673909,-2.75079071295314,5.9));
#10336=CARTESIAN_POINT('',(1.49184997416615,-1.19714262038019,6.8));
#10337=CARTESIAN_POINT('Origin',(1.24264068711928,-3.,6.8));
#10338=CARTESIAN_POINT('',(1.49184997416615,-1.19714262038019,5.9));
#10339=CARTESIAN_POINT('Origin',(1.24264068711929,3.,5.9));
#10340=CARTESIAN_POINT('',(1.49184997416615,1.19714262038019,6.));
#10341=CARTESIAN_POINT('',(3.04549806673909,2.75079071295314,6.));
#10342=CARTESIAN_POINT('Origin',(1.24264068711929,3.,6.));
#10343=CARTESIAN_POINT('',(1.49184997416615,1.19714262038019,6.8));
#10344=CARTESIAN_POINT('',(1.49184997416615,1.19714262038019,5.9));
#10345=CARTESIAN_POINT('',(3.04549806673909,2.75079071295314,6.8));
#10346=CARTESIAN_POINT('Origin',(1.24264068711929,3.,6.8));
#10347=CARTESIAN_POINT('',(3.04549806673909,2.75079071295314,5.9));
#10348=CARTESIAN_POINT('Origin',(7.24264068711929,3.,5.9));
#10349=CARTESIAN_POINT('',(5.43978330749948,2.75079071295314,6.));
#10350=CARTESIAN_POINT('',(6.99343140007243,1.19714262038019,6.));
#10351=CARTESIAN_POINT('Origin',(7.24264068711929,3.,6.));
#10352=CARTESIAN_POINT('',(5.43978330749948,2.75079071295314,6.8));
#10353=CARTESIAN_POINT('',(5.43978330749948,2.75079071295314,5.9));
#10354=CARTESIAN_POINT('',(6.99343140007243,1.19714262038019,6.8));
#10355=CARTESIAN_POINT('Origin',(7.24264068711929,3.,6.8));
#10356=CARTESIAN_POINT('',(6.99343140007243,1.19714262038019,5.9));
#10357=CARTESIAN_POINT('Origin',(7.24264068711929,-3.,5.9));
#10358=CARTESIAN_POINT('',(6.99343140007242,-1.19714262038019,6.8));
#10359=CARTESIAN_POINT('',(6.99343140007242,-1.19714262038019,6.));
#10360=CARTESIAN_POINT('',(6.99343140007243,-1.19714262038019,5.9));
#10361=CARTESIAN_POINT('',(5.43978330749948,-2.75079071295314,6.8));
#10362=CARTESIAN_POINT('Origin',(7.24264068711929,-3.,6.8));
#10363=CARTESIAN_POINT('',(5.43978330749948,-2.75079071295314,6.));
#10364=CARTESIAN_POINT('',(5.43978330749948,-2.75079071295314,5.9));
#10365=CARTESIAN_POINT('Origin',(7.24264068711929,-3.,6.));
#10366=CARTESIAN_POINT('Origin',(4.24264068711929,0.,6.));
#10367=CARTESIAN_POINT('',(3.81264068711929,-2.96902340846279,6.));
#10368=CARTESIAN_POINT('Origin',(4.24264068711929,0.,6.));
#10369=CARTESIAN_POINT('',(3.81264068711929,-2.96902340846279,6.8));
#10370=CARTESIAN_POINT('',(3.81264068711929,-2.96902340846279,6.));
#10371=CARTESIAN_POINT('Origin',(4.24264068711929,0.,6.8));
#10372=CARTESIAN_POINT('Origin',(4.24264068711929,0.,6.));
#10373=CARTESIAN_POINT('',(1.2736172786565,0.43,6.));
#10374=CARTESIAN_POINT('Origin',(4.24264068711929,0.,6.));
#10375=CARTESIAN_POINT('',(1.2736172786565,0.43,6.8));
#10376=CARTESIAN_POINT('',(1.2736172786565,0.43,6.));
#10377=CARTESIAN_POINT('Origin',(4.24264068711929,0.,6.8));
#10378=CARTESIAN_POINT('Origin',(4.24264068711929,0.,6.));
#10379=CARTESIAN_POINT('',(4.67264068711929,2.96902340846279,6.));
#10380=CARTESIAN_POINT('Origin',(4.24264068711929,0.,6.));
#10381=CARTESIAN_POINT('',(4.67264068711929,2.96902340846279,6.8));
#10382=CARTESIAN_POINT('',(4.67264068711929,2.96902340846279,6.));
#10383=CARTESIAN_POINT('Origin',(4.24264068711929,0.,6.8));
#10384=CARTESIAN_POINT('Origin',(4.24264068711929,0.,6.8));
#10385=CARTESIAN_POINT('',(3.81264068711929,-2.6,6.8));
#10386=CARTESIAN_POINT('',(3.81264068711929,-1.3,6.8));
#10387=CARTESIAN_POINT('',(3.92264068711928,-2.6,6.8));
#10388=CARTESIAN_POINT('',(4.45764068711929,-2.6,6.8));
#10389=CARTESIAN_POINT('',(3.92264068711928,-1.,6.8));
#10390=CARTESIAN_POINT('',(3.92264068711929,-0.5,6.8));
#10391=CARTESIAN_POINT('',(4.56264068711929,-1.,6.8));
#10392=CARTESIAN_POINT('Origin',(4.24264068711929,-1.,6.8));
#10393=CARTESIAN_POINT('',(4.56264068711929,-2.6,6.8));
#10394=CARTESIAN_POINT('',(4.56264068711929,-1.8,6.8));
#10395=CARTESIAN_POINT('',(4.67264068711928,-2.6,6.8));
#10396=CARTESIAN_POINT('',(4.45764068711929,-2.6,6.8));
#10397=CARTESIAN_POINT('',(4.67264068711928,-2.96902340846279,6.8));
#10398=CARTESIAN_POINT('',(4.67264068711929,-1.8,6.8));
#10399=CARTESIAN_POINT('Origin',(4.24264068711929,0.,6.8));
#10400=CARTESIAN_POINT('',(7.21166409558207,-0.43,6.8));
#10401=CARTESIAN_POINT('Origin',(4.24264068711929,0.,6.8));
#10402=CARTESIAN_POINT('',(6.84264068711929,-0.43,6.8));
#10403=CARTESIAN_POINT('',(5.54264068711929,-0.43,6.8));
#10404=CARTESIAN_POINT('',(6.84264068711929,-0.32,6.8));
#10405=CARTESIAN_POINT('',(6.84264068711929,0.215,6.8));
#10406=CARTESIAN_POINT('',(5.24264068711929,-0.32,6.8));
#10407=CARTESIAN_POINT('',(4.74264068711929,-0.32,6.8));
#10408=CARTESIAN_POINT('',(5.24264068711929,0.32,6.8));
#10409=CARTESIAN_POINT('Origin',(5.24264068711929,0.,6.8));
#10410=CARTESIAN_POINT('',(6.84264068711929,0.32,6.8));
#10411=CARTESIAN_POINT('',(6.04264068711929,0.32,6.8));
#10412=CARTESIAN_POINT('',(6.84264068711929,0.43,6.8));
#10413=CARTESIAN_POINT('',(6.84264068711929,0.215,6.8));
#10414=CARTESIAN_POINT('',(7.21166409558207,0.43,6.8));
#10415=CARTESIAN_POINT('',(6.04264068711929,0.43,6.8));
#10416=CARTESIAN_POINT('Origin',(4.24264068711929,0.,6.8));
#10417=CARTESIAN_POINT('',(4.67264068711929,2.6,6.8));
#10418=CARTESIAN_POINT('',(4.67264068711929,1.3,6.8));
#10419=CARTESIAN_POINT('',(4.56264068711929,2.6,6.8));
#10420=CARTESIAN_POINT('',(4.02764068711929,2.6,6.8));
#10421=CARTESIAN_POINT('',(4.56264068711929,1.,6.8));
#10422=CARTESIAN_POINT('',(4.56264068711929,0.5,6.8));
#10423=CARTESIAN_POINT('',(3.92264068711928,1.,6.8));
#10424=CARTESIAN_POINT('Origin',(4.24264068711929,1.,6.8));
#10425=CARTESIAN_POINT('',(3.92264068711929,2.6,6.8));
#10426=CARTESIAN_POINT('',(3.92264068711929,1.8,6.8));
#10427=CARTESIAN_POINT('',(3.81264068711929,2.6,6.8));
#10428=CARTESIAN_POINT('',(4.02764068711929,2.6,6.8));
#10429=CARTESIAN_POINT('',(3.81264068711929,2.96902340846279,6.8));
#10430=CARTESIAN_POINT('',(3.81264068711929,1.8,6.8));
#10431=CARTESIAN_POINT('Origin',(4.24264068711929,0.,6.8));
#10432=CARTESIAN_POINT('',(1.64264068711929,0.43,6.8));
#10433=CARTESIAN_POINT('',(2.94264068711929,0.43,6.8));
#10434=CARTESIAN_POINT('',(1.64264068711929,0.32,6.8));
#10435=CARTESIAN_POINT('',(1.64264068711929,-0.215,6.8));
#10436=CARTESIAN_POINT('',(3.24264068711929,0.32,6.8));
#10437=CARTESIAN_POINT('',(3.74264068711929,0.32,6.8));
#10438=CARTESIAN_POINT('',(3.24264068711929,-0.32,6.8));
#10439=CARTESIAN_POINT('Origin',(3.24264068711929,1.22464679914735E-16,
6.8));
#10440=CARTESIAN_POINT('',(1.64264068711929,-0.32,6.8));
#10441=CARTESIAN_POINT('',(2.44264068711929,-0.32,6.8));
#10442=CARTESIAN_POINT('',(1.64264068711929,-0.43,6.8));
#10443=CARTESIAN_POINT('',(1.64264068711929,-0.215,6.8));
#10444=CARTESIAN_POINT('',(1.2736172786565,-0.43,6.8));
#10445=CARTESIAN_POINT('',(2.44264068711929,-0.43,6.8));
#10446=CARTESIAN_POINT('Origin',(4.24264068711929,0.,6.8));
#10447=CARTESIAN_POINT('Origin',(4.24264068711929,0.,6.));
#10448=CARTESIAN_POINT('',(7.21166409558207,-0.43,6.));
#10449=CARTESIAN_POINT('Origin',(4.24264068711929,0.,6.));
#10450=CARTESIAN_POINT('',(7.21166409558207,-0.43,6.));
#10451=CARTESIAN_POINT('Origin',(4.24264068711929,0.,6.));
#10452=CARTESIAN_POINT('',(4.67264068711928,-2.96902340846279,6.));
#10453=CARTESIAN_POINT('',(4.67264068711928,-2.96902340846279,6.));
#10454=CARTESIAN_POINT('Origin',(4.24264068711929,0.,6.));
#10455=CARTESIAN_POINT('Origin',(4.67264068711928,-3.6,5.9));
#10456=CARTESIAN_POINT('',(4.67264068711928,-2.6,6.));
#10457=CARTESIAN_POINT('',(4.67264068711928,-2.6,5.9));
#10458=CARTESIAN_POINT('',(4.67264068711929,-1.8,6.));
#10459=CARTESIAN_POINT('Origin',(4.67264068711928,-2.6,5.9));
#10460=CARTESIAN_POINT('',(4.56264068711929,-2.6,6.));
#10461=CARTESIAN_POINT('',(4.56264068711929,-2.6,5.9));
#10462=CARTESIAN_POINT('',(4.45764068711929,-2.6,6.));
#10463=CARTESIAN_POINT('Origin',(4.67264068711928,-2.6,5.9));
#10464=CARTESIAN_POINT('',(3.81264068711929,-2.6,6.));
#10465=CARTESIAN_POINT('',(3.81264068711929,-2.6,5.9));
#10466=CARTESIAN_POINT('',(3.92264068711928,-2.6,6.));
#10467=CARTESIAN_POINT('',(4.45764068711929,-2.6,6.));
#10468=CARTESIAN_POINT('',(3.92264068711928,-2.6,5.9));
#10469=CARTESIAN_POINT('Origin',(3.81264068711929,-2.6,5.9));
#10470=CARTESIAN_POINT('',(3.81264068711929,-1.3,6.));
#10471=CARTESIAN_POINT('Origin',(3.92264068711928,-1.,5.9));
#10472=CARTESIAN_POINT('',(3.92264068711928,-1.,6.));
#10473=CARTESIAN_POINT('',(3.92264068711929,-0.5,6.));
#10474=CARTESIAN_POINT('',(3.92264068711928,-1.,5.9));
#10475=CARTESIAN_POINT('Origin',(4.24264068711929,0.,6.));
#10476=CARTESIAN_POINT('',(1.2736172786565,-0.43,6.));
#10477=CARTESIAN_POINT('Origin',(4.24264068711929,0.,6.));
#10478=CARTESIAN_POINT('',(1.64264068711929,-0.43,6.));
#10479=CARTESIAN_POINT('',(2.44264068711929,-0.43,6.));
#10480=CARTESIAN_POINT('',(1.64264068711929,-0.32,6.));
#10481=CARTESIAN_POINT('',(1.64264068711929,-0.215,6.));
#10482=CARTESIAN_POINT('',(3.24264068711929,-0.32,6.));
#10483=CARTESIAN_POINT('',(2.44264068711929,-0.32,6.));
#10484=CARTESIAN_POINT('',(3.54884068711929,-0.0929599913941466,6.));
#10485=CARTESIAN_POINT('Origin',(3.24264068711929,1.22464679914735E-16,
6.));
#10486=CARTESIAN_POINT('',(4.14968069572514,-0.6938,6.));
#10487=CARTESIAN_POINT('Origin',(4.24264068711929,0.,6.));
#10488=CARTESIAN_POINT('Origin',(4.24264068711929,-1.,6.));
#10489=CARTESIAN_POINT('Origin',(4.24264068711929,0.,6.));
#10490=CARTESIAN_POINT('',(4.56264068711929,-1.,6.));
#10491=CARTESIAN_POINT('',(4.56264068711929,-1.8,6.));
#10492=CARTESIAN_POINT('',(4.33560067851344,-0.6938,6.));
#10493=CARTESIAN_POINT('Origin',(4.24264068711929,-1.,6.));
#10494=CARTESIAN_POINT('',(4.93644068711929,-0.0929599913941494,6.));
#10495=CARTESIAN_POINT('Origin',(4.24264068711929,0.,6.));
#10496=CARTESIAN_POINT('',(5.24264068711929,-0.32,6.));
#10497=CARTESIAN_POINT('Origin',(5.24264068711929,0.,6.));
#10498=CARTESIAN_POINT('',(6.84264068711929,-0.32,6.));
#10499=CARTESIAN_POINT('',(4.74264068711929,-0.32,6.));
#10500=CARTESIAN_POINT('',(6.84264068711929,-0.43,6.));
#10501=CARTESIAN_POINT('',(6.84264068711929,0.215,6.));
#10502=CARTESIAN_POINT('',(5.54264068711929,-0.43,6.));
#10503=CARTESIAN_POINT('Origin',(4.24264068711929,-1.,5.9));
#10504=CARTESIAN_POINT('',(4.33560067851343,-0.6938,5.9));
#10505=CARTESIAN_POINT('',(4.14968069572514,-0.6938,5.9));
#10506=CARTESIAN_POINT('Origin',(4.24264068711929,0.,5.9));
#10507=CARTESIAN_POINT('Origin',(4.24264068711929,-1.,5.9));
#10508=CARTESIAN_POINT('Origin',(4.24264068711929,-1.,5.9));
#10509=CARTESIAN_POINT('',(4.33560067851343,-0.6938,5.9));
#10510=CARTESIAN_POINT('',(4.56264068711929,-1.,5.9));
#10511=CARTESIAN_POINT('',(4.14968069572514,-0.6938,5.9));
#10512=CARTESIAN_POINT('Origin',(4.24264068711929,0.,2.95));
#10513=CARTESIAN_POINT('',(3.54884068711929,-0.0929599913941465,5.9));
#10514=CARTESIAN_POINT('',(3.54884068711929,-0.0929599913941465,5.9));
#10515=CARTESIAN_POINT('',(3.54264068711929,-8.57252759403147E-17,5.9));
#10516=CARTESIAN_POINT('Origin',(4.24264068711929,0.,5.9));
#10517=CARTESIAN_POINT('',(3.54264068711929,-8.57252759403147E-17,2.95));
#10518=CARTESIAN_POINT('',(3.54264068711929,-8.57252759403147E-17,2.95));
#10519=CARTESIAN_POINT('Origin',(4.24264068711929,0.,2.95));
#10520=CARTESIAN_POINT('',(3.54884068711929,0.0929599913941467,5.9));
#10521=CARTESIAN_POINT('Origin',(4.24264068711929,0.,5.9));
#10522=CARTESIAN_POINT('',(3.54884068711929,0.0929599913941468,6.));
#10523=CARTESIAN_POINT('',(3.54884068711929,0.0929599913941467,5.9));
#10524=CARTESIAN_POINT('',(4.14968069572514,0.6938,6.));
#10525=CARTESIAN_POINT('Origin',(4.24264068711929,0.,6.));
#10526=CARTESIAN_POINT('',(4.14968069572514,0.6938,5.9));
#10527=CARTESIAN_POINT('',(4.14968069572514,0.6938,5.9));
#10528=CARTESIAN_POINT('',(4.33560067851343,0.6938,5.9));
#10529=CARTESIAN_POINT('Origin',(4.24264068711929,0.,5.9));
#10530=CARTESIAN_POINT('',(4.33560067851344,0.6938,6.));
#10531=CARTESIAN_POINT('',(4.33560067851343,0.6938,5.9));
#10532=CARTESIAN_POINT('',(4.93644068711929,0.0929599913941494,6.));
#10533=CARTESIAN_POINT('Origin',(4.24264068711929,0.,6.));
#10534=CARTESIAN_POINT('',(4.93644068711929,0.0929599913941487,5.9));
#10535=CARTESIAN_POINT('',(4.93644068711929,0.0929599913941487,5.9));
#10536=CARTESIAN_POINT('',(4.93644068711929,-0.0929599913941487,5.9));
#10537=CARTESIAN_POINT('Origin',(4.24264068711929,0.,5.9));
#10538=CARTESIAN_POINT('',(4.93644068711929,-0.0929599913941487,5.9));
#10539=CARTESIAN_POINT('Origin',(4.56264068711929,-3.6,5.9));
#10540=CARTESIAN_POINT('Origin',(4.24264068711929,0.,6.));
#10541=CARTESIAN_POINT('',(1.2736172786565,-0.43,6.));
#10542=CARTESIAN_POINT('Origin',(0.642640687119285,-0.43,5.9));
#10543=CARTESIAN_POINT('',(1.64264068711929,-0.43,5.9));
#10544=CARTESIAN_POINT('Origin',(1.64264068711929,-0.43,5.9));
#10545=CARTESIAN_POINT('',(1.64264068711929,-0.32,5.9));
#10546=CARTESIAN_POINT('Origin',(1.64264068711929,-0.43,5.9));
#10547=CARTESIAN_POINT('',(1.64264068711929,0.43,6.));
#10548=CARTESIAN_POINT('',(1.64264068711929,0.43,5.9));
#10549=CARTESIAN_POINT('',(1.64264068711929,0.32,6.));
#10550=CARTESIAN_POINT('',(1.64264068711929,-0.215,6.));
#10551=CARTESIAN_POINT('',(1.64264068711929,0.32,5.9));
#10552=CARTESIAN_POINT('Origin',(1.64264068711929,0.43,5.9));
#10553=CARTESIAN_POINT('',(2.94264068711929,0.43,6.));
#10554=CARTESIAN_POINT('Origin',(3.24264068711929,0.32,5.9));
#10555=CARTESIAN_POINT('',(3.24264068711929,0.32,6.));
#10556=CARTESIAN_POINT('',(3.74264068711929,0.32,6.));
#10557=CARTESIAN_POINT('',(3.24264068711929,0.32,5.9));
#10558=CARTESIAN_POINT('Origin',(4.24264068711929,0.,6.));
#10559=CARTESIAN_POINT('',(3.81264068711929,2.96902340846279,6.));
#10560=CARTESIAN_POINT('Origin',(4.24264068711929,0.,6.));
#10561=CARTESIAN_POINT('',(3.81264068711929,2.6,6.));
#10562=CARTESIAN_POINT('',(3.81264068711929,1.8,6.));
#10563=CARTESIAN_POINT('',(3.92264068711929,2.6,6.));
#10564=CARTESIAN_POINT('',(4.02764068711929,2.6,6.));
#10565=CARTESIAN_POINT('',(3.92264068711928,1.,6.));
#10566=CARTESIAN_POINT('',(3.92264068711929,1.8,6.));
#10567=CARTESIAN_POINT('Origin',(4.24264068711929,1.,6.));
#10568=CARTESIAN_POINT('Origin',(3.24264068711929,1.22464679914735E-16,
6.));
#10569=CARTESIAN_POINT('Origin',(3.24264068711929,1.11022302462516E-16,
5.9));
#10570=CARTESIAN_POINT('Origin',(3.24264068711929,1.22464679914735E-16,
5.9));
#10571=CARTESIAN_POINT('Origin',(3.24264068711929,1.22464679914735E-16,
5.9));
#10572=CARTESIAN_POINT('',(3.24264068711929,-0.32,5.9));
#10573=CARTESIAN_POINT('Origin',(0.642640687119285,-0.32,5.9));
#10574=CARTESIAN_POINT('Origin',(4.24264068711929,0.,6.));
#10575=CARTESIAN_POINT('',(3.81264068711929,2.96902340846279,6.));
#10576=CARTESIAN_POINT('Origin',(3.81264068711929,3.6,5.9));
#10577=CARTESIAN_POINT('',(3.81264068711929,2.6,5.9));
#10578=CARTESIAN_POINT('Origin',(3.81264068711929,2.6,5.9));
#10579=CARTESIAN_POINT('',(3.92264068711928,2.6,5.9));
#10580=CARTESIAN_POINT('Origin',(3.81264068711929,2.6,5.9));
#10581=CARTESIAN_POINT('',(4.67264068711929,2.6,6.));
#10582=CARTESIAN_POINT('',(4.67264068711929,2.6,5.9));
#10583=CARTESIAN_POINT('',(4.56264068711929,2.6,6.));
#10584=CARTESIAN_POINT('',(4.02764068711929,2.6,6.));
#10585=CARTESIAN_POINT('',(4.56264068711929,2.6,5.9));
#10586=CARTESIAN_POINT('Origin',(4.67264068711929,2.6,5.9));
#10587=CARTESIAN_POINT('',(4.67264068711929,1.3,6.));
#10588=CARTESIAN_POINT('Origin',(4.56264068711929,1.,5.9));
#10589=CARTESIAN_POINT('',(4.56264068711929,1.,6.));
#10590=CARTESIAN_POINT('',(4.56264068711929,0.5,6.));
#10591=CARTESIAN_POINT('',(4.56264068711929,1.,5.9));
#10592=CARTESIAN_POINT('Origin',(4.24264068711929,0.,6.));
#10593=CARTESIAN_POINT('',(7.21166409558207,0.43,6.));
#10594=CARTESIAN_POINT('Origin',(4.24264068711929,0.,6.));
#10595=CARTESIAN_POINT('',(6.84264068711929,0.43,6.));
#10596=CARTESIAN_POINT('',(6.04264068711929,0.43,6.));
#10597=CARTESIAN_POINT('',(6.84264068711929,0.32,6.));
#10598=CARTESIAN_POINT('',(6.84264068711929,0.215,6.));
#10599=CARTESIAN_POINT('',(5.24264068711929,0.32,6.));
#10600=CARTESIAN_POINT('',(6.04264068711929,0.32,6.));
#10601=CARTESIAN_POINT('Origin',(5.24264068711929,0.,6.));
#10602=CARTESIAN_POINT('Origin',(4.24264068711929,1.,6.));
#10603=CARTESIAN_POINT('Origin',(4.24264068711929,1.,5.9));
#10604=CARTESIAN_POINT('Origin',(4.24264068711929,1.,5.9));
#10605=CARTESIAN_POINT('Origin',(4.24264068711929,1.,5.9));
#10606=CARTESIAN_POINT('',(3.92264068711928,1.,5.9));
#10607=CARTESIAN_POINT('Origin',(3.92264068711928,3.6,5.9));
#10608=CARTESIAN_POINT('Origin',(4.24264068711929,0.,6.));
#10609=CARTESIAN_POINT('',(7.21166409558207,0.43,6.));
#10610=CARTESIAN_POINT('Origin',(7.84264068711929,0.43,5.9));
#10611=CARTESIAN_POINT('',(6.84264068711929,0.43,5.9));
#10612=CARTESIAN_POINT('Origin',(6.84264068711929,-0.43,5.9));
#10613=CARTESIAN_POINT('',(6.84264068711929,-0.43,5.9));
#10614=CARTESIAN_POINT('Origin',(6.84264068711929,0.43,5.9));
#10615=CARTESIAN_POINT('',(6.84264068711929,-0.32,5.9));
#10616=CARTESIAN_POINT('Origin',(6.84264068711929,0.43,5.9));
#10617=CARTESIAN_POINT('',(6.84264068711929,0.32,5.9));
#10618=CARTESIAN_POINT('Origin',(5.24264068711929,0.,5.9));
#10619=CARTESIAN_POINT('Origin',(5.24264068711929,0.,5.9));
#10620=CARTESIAN_POINT('Origin',(5.24264068711929,0.,5.9));
#10621=CARTESIAN_POINT('',(5.24264068711929,0.32,5.9));
#10622=CARTESIAN_POINT('',(5.24264068711929,-0.32,5.9));
#10623=CARTESIAN_POINT('Origin',(7.84264068711929,0.32,5.9));
#10624=CARTESIAN_POINT('Origin',(5.24264068711929,-0.32,5.9));
#10625=CARTESIAN_POINT('Origin',(4.24264068711929,0.,2.95));
#10626=CARTESIAN_POINT('',(3.74264068711929,6.12323399573677E-17,2.95));
#10627=CARTESIAN_POINT('Origin',(4.24264068711929,0.,2.95));
#10628=CARTESIAN_POINT('Origin',(4.24264068711929,0.,1.));
#10629=CARTESIAN_POINT('',(3.74264068711929,-6.12323399573677E-17,1.));
#10630=CARTESIAN_POINT('',(3.74264068711929,-6.12323399573677E-17,1.));
#10631=CARTESIAN_POINT('Origin',(4.24264068711929,0.,1.));
#10632=CARTESIAN_POINT('Origin',(4.24264068711929,0.,1.));
#10633=CARTESIAN_POINT('',(0.,0.,0.));
#10634=CARTESIAN_POINT('Origin',(4.24264068711929,0.,1.8));
#10635=CARTESIAN_POINT('',(3.73764068711929,-6.18446633569413E-17,2.05));
#10636=CARTESIAN_POINT('Origin',(4.24264068711929,0.,2.05));
#10637=CARTESIAN_POINT('',(3.73764068711929,-6.18446633569413E-17,1.8));
#10638=CARTESIAN_POINT('',(3.73764068711929,-6.18446633569413E-17,1.8));
#10639=CARTESIAN_POINT('Origin',(4.24264068711929,0.,1.8));
#10640=CARTESIAN_POINT('Origin',(4.24264068711929,0.,1.8));
#10641=CARTESIAN_POINT('',(3.54264068711929,-8.57252759403147E-17,2.05));
#10642=CARTESIAN_POINT('Origin',(4.24264068711929,0.,2.05));
#10643=CARTESIAN_POINT('',(3.54264068711929,-8.57252759403147E-17,1.8));
#10644=CARTESIAN_POINT('',(3.54264068711929,-8.57252759403147E-17,1.8));
#10645=CARTESIAN_POINT('Origin',(4.24264068711929,0.,1.8));
#10646=CARTESIAN_POINT('Origin',(4.24264068711929,0.,2.05));
#10647=CARTESIAN_POINT('Origin',(4.24264068711929,0.,1.8));
#10648=CARTESIAN_POINT('',(0.,0.,0.));
#10649=CARTESIAN_POINT('Origin',(4.24264068711929,-0.49,1.4));
#10650=CARTESIAN_POINT('',(4.12047276989058,-0.49,1.51090536506409));
#10651=CARTESIAN_POINT('',(4.12047276989058,-0.49,1.28909463493591));
#10652=CARTESIAN_POINT('',(4.12047276989058,-0.49,1.));
#10653=CARTESIAN_POINT('',(4.07764068711929,-0.49,1.4));
#10654=CARTESIAN_POINT('Origin',(4.24264068711929,-0.49,1.4));
#10655=CARTESIAN_POINT('Origin',(4.24264068711929,-0.49,1.4));
#10656=CARTESIAN_POINT('Origin',(4.24264068711929,-1.,1.4));
#10657=CARTESIAN_POINT('',(4.07764068711929,-0.884745726183518,1.4));
#10658=CARTESIAN_POINT('Ctrl Pts',(4.07764068711929,-0.884745726183518,
1.4));
#10659=CARTESIAN_POINT('Ctrl Pts',(4.07764068711929,-0.884745726183518,
1.42076875940744));
#10660=CARTESIAN_POINT('Ctrl Pts',(4.0818009681117,-0.885552759505265,1.44288889507334));
#10661=CARTESIAN_POINT('Ctrl Pts',(4.0986542169026,-0.888448648150043,1.48352706263377));
#10662=CARTESIAN_POINT('Ctrl Pts',(4.1113446933051,-0.890493604851638,1.50204924397737));
#10663=CARTESIAN_POINT('Ctrl Pts',(4.14059086811116,-0.894317234323941,
1.53129541878344));
#10664=CARTESIAN_POINT('Ctrl Pts',(4.1591132950286,-0.896347088899543,1.54398634598358));
#10665=CARTESIAN_POINT('Ctrl Pts',(4.19975231102587,-0.899208271860583,
1.56083992183864));
#10666=CARTESIAN_POINT('Ctrl Pts',(4.22187274439578,-0.9,1.565));
#10667=CARTESIAN_POINT('Ctrl Pts',(4.26340862984279,-0.9,1.565));
#10668=CARTESIAN_POINT('Ctrl Pts',(4.2855290632127,-0.899208271860583,1.56083992183864));
#10669=CARTESIAN_POINT('Ctrl Pts',(4.32616807920997,-0.896347088899543,
1.54398634598358));
#10670=CARTESIAN_POINT('Ctrl Pts',(4.34469050612741,-0.894317234323941,
1.53129541878344));
#10671=CARTESIAN_POINT('Ctrl Pts',(4.37393668093347,-0.890493604851638,
1.50204924397737));
#10672=CARTESIAN_POINT('Ctrl Pts',(4.38662715733598,-0.888448648150043,
1.48352706263377));
#10673=CARTESIAN_POINT('Ctrl Pts',(4.40348040612687,-0.885552759505265,
1.44288889507334));
#10674=CARTESIAN_POINT('Ctrl Pts',(4.40764068711929,-0.884745726183518,
1.42076875940744));
#10675=CARTESIAN_POINT('Ctrl Pts',(4.40764068711929,-0.884745726183518,
1.37923124059256));
#10676=CARTESIAN_POINT('Ctrl Pts',(4.40348040612687,-0.885552759505265,
1.35711110492666));
#10677=CARTESIAN_POINT('Ctrl Pts',(4.38662715733598,-0.888448648150043,
1.31647293736623));
#10678=CARTESIAN_POINT('Ctrl Pts',(4.37393668093347,-0.890493604851638,
1.29795075602263));
#10679=CARTESIAN_POINT('Ctrl Pts',(4.34469050612741,-0.894317234323941,
1.26870458121656));
#10680=CARTESIAN_POINT('Ctrl Pts',(4.32616807920997,-0.896347088899543,
1.25601365401642));
#10681=CARTESIAN_POINT('Ctrl Pts',(4.2855290632127,-0.899208271860583,1.23916007816136));
#10682=CARTESIAN_POINT('Ctrl Pts',(4.26340862984279,-0.9,1.235));
#10683=CARTESIAN_POINT('Ctrl Pts',(4.22187274439578,-0.9,1.235));
#10684=CARTESIAN_POINT('Ctrl Pts',(4.19975231102587,-0.899208271860583,
1.23916007816136));
#10685=CARTESIAN_POINT('Ctrl Pts',(4.1591132950286,-0.896347088899543,1.25601365401642));
#10686=CARTESIAN_POINT('Ctrl Pts',(4.14059086811116,-0.894317234323941,
1.26870458121656));
#10687=CARTESIAN_POINT('Ctrl Pts',(4.1113446933051,-0.890493604851638,1.29795075602263));
#10688=CARTESIAN_POINT('Ctrl Pts',(4.0986542169026,-0.888448648150043,1.31647293736623));
#10689=CARTESIAN_POINT('Ctrl Pts',(4.0818009681117,-0.885552759505265,1.35711110492666));
#10690=CARTESIAN_POINT('Ctrl Pts',(4.07764068711929,-0.884745726183518,
1.37923124059256));
#10691=CARTESIAN_POINT('Ctrl Pts',(4.07764068711929,-0.884745726183518,
1.4));
#10692=CARTESIAN_POINT('',(4.07764068711929,-1.,1.4));
#10693=CARTESIAN_POINT('',(4.36480860434799,-0.49,1.51090536506409));
#10694=CARTESIAN_POINT('Ctrl Pts',(4.36480860434799,-0.49,1.51090536506409));
#10695=CARTESIAN_POINT('Ctrl Pts',(4.36300960074558,-0.490448531679987,
1.51288705930464));
#10696=CARTESIAN_POINT('Ctrl Pts',(4.36117558368452,-0.490895245371684,
1.51481034122633));
#10697=CARTESIAN_POINT('Ctrl Pts',(4.34475268013864,-0.494795015531646,
1.5312332447722));
#10698=CARTESIAN_POINT('Ctrl Pts',(4.32630040214172,-0.498442514607594,
1.54390845611142));
#10699=CARTESIAN_POINT('Ctrl Pts',(4.28569028316644,-0.50357781976106,1.56079590960766));
#10700=CARTESIAN_POINT('Ctrl Pts',(4.26352078145003,-0.505,1.565));
#10701=CARTESIAN_POINT('Ctrl Pts',(4.22176059278855,-0.505,1.565));
#10702=CARTESIAN_POINT('Ctrl Pts',(4.19959109107213,-0.50357781976106,1.56079590960766));
#10703=CARTESIAN_POINT('Ctrl Pts',(4.15898097209685,-0.498442514607594,
1.54390845611142));
#10704=CARTESIAN_POINT('Ctrl Pts',(4.14052869409993,-0.494795015531646,
1.5312332447722));
#10705=CARTESIAN_POINT('Ctrl Pts',(4.12410579055406,-0.490895245371684,
1.51481034122633));
#10706=CARTESIAN_POINT('Ctrl Pts',(4.12227177349299,-0.490448531679987,
1.51288705930464));
#10707=CARTESIAN_POINT('Ctrl Pts',(4.12047276989058,-0.49,1.51090536506409));
#10708=CARTESIAN_POINT('',(4.36480860434799,-0.49,1.28909463493591));
#10709=CARTESIAN_POINT('Origin',(4.24264068711929,-0.49,1.4));
#10710=CARTESIAN_POINT('Ctrl Pts',(4.12047276989058,-0.49,1.28909463493591));
#10711=CARTESIAN_POINT('Ctrl Pts',(4.12227177349299,-0.490448531679987,
1.28711294069536));
#10712=CARTESIAN_POINT('Ctrl Pts',(4.12410579055406,-0.490895245371684,
1.28518965877367));
#10713=CARTESIAN_POINT('Ctrl Pts',(4.14052869409993,-0.494795015531646,
1.2687667552278));
#10714=CARTESIAN_POINT('Ctrl Pts',(4.15898097209685,-0.498442514607594,
1.25609154388858));
#10715=CARTESIAN_POINT('Ctrl Pts',(4.19959109107213,-0.50357781976106,1.23920409039234));
#10716=CARTESIAN_POINT('Ctrl Pts',(4.22176059278855,-0.505,1.235));
#10717=CARTESIAN_POINT('Ctrl Pts',(4.26352078145003,-0.505,1.235));
#10718=CARTESIAN_POINT('Ctrl Pts',(4.28569028316644,-0.50357781976106,1.23920409039234));
#10719=CARTESIAN_POINT('Ctrl Pts',(4.32630040214172,-0.498442514607594,
1.25609154388858));
#10720=CARTESIAN_POINT('Ctrl Pts',(4.34475268013864,-0.494795015531646,
1.2687667552278));
#10721=CARTESIAN_POINT('Ctrl Pts',(4.36117558368452,-0.490895245371684,
1.28518965877367));
#10722=CARTESIAN_POINT('Ctrl Pts',(4.36300960074558,-0.490448531679987,
1.28711294069536));
#10723=CARTESIAN_POINT('Ctrl Pts',(4.36480860434799,-0.49,1.28909463493591));
#10724=CARTESIAN_POINT('Origin',(4.24264068711929,-0.49,1.4));
#10725=CARTESIAN_POINT('',(4.36480860434799,-0.49,1.));
#10726=CARTESIAN_POINT('Origin',(3.75264069,0.,1.4));
#10727=CARTESIAN_POINT('',(3.75264069,0.122167928782887,1.51090535233657));
#10728=CARTESIAN_POINT('',(3.75264069,0.122167928782887,1.28909464766343));
#10729=CARTESIAN_POINT('',(3.75264069,0.122167928782887,1.));
#10730=CARTESIAN_POINT('Origin',(3.75264069,0.,1.4));
#10731=CARTESIAN_POINT('Origin',(3.24264069,0.,1.4));
#10732=CARTESIAN_POINT('',(3.35789496093577,0.165,1.4));
#10733=CARTESIAN_POINT('',(3.34264068711929,-2.02066721859313E-17,1.565));
#10734=CARTESIAN_POINT('Ctrl Pts',(3.35789496093577,0.165,1.4));
#10735=CARTESIAN_POINT('Ctrl Pts',(3.35789496093577,0.165,1.42076875940744));
#10736=CARTESIAN_POINT('Ctrl Pts',(3.35708792761402,0.160839719007584,1.44288889507334));
#10737=CARTESIAN_POINT('Ctrl Pts',(3.35419203896924,0.143986470216691,1.48352706263377));
#10738=CARTESIAN_POINT('Ctrl Pts',(3.35214708226765,0.131295993814186,1.50204924397737));
#10739=CARTESIAN_POINT('Ctrl Pts',(3.34832345279534,0.102049819008125,1.53129541878344));
#10740=CARTESIAN_POINT('Ctrl Pts',(3.34629359821974,0.0835273920906824,
1.54398634598358));
#10741=CARTESIAN_POINT('Ctrl Pts',(3.3434324152587,0.0428883760934127,1.56083992183864));
#10742=CARTESIAN_POINT('Ctrl Pts',(3.34264068711929,0.0207679427235068,
1.565));
#10743=CARTESIAN_POINT('Ctrl Pts',(3.34264068711929,2.77555756156289E-17,
1.565));
#10744=CARTESIAN_POINT('',(3.34264068711929,-7.59257876733526E-17,1.235));
#10745=CARTESIAN_POINT('Ctrl Pts',(3.34264068711929,-4.16333634234434E-17,
1.235));
#10746=CARTESIAN_POINT('Ctrl Pts',(3.34264068711929,0.0207679427235068,
1.235));
#10747=CARTESIAN_POINT('Ctrl Pts',(3.3434324152587,0.0428883760934127,1.23916007816136));
#10748=CARTESIAN_POINT('Ctrl Pts',(3.34629359821974,0.0835273920906823,
1.25601365401642));
#10749=CARTESIAN_POINT('Ctrl Pts',(3.34832345279534,0.102049819008125,1.26870458121656));
#10750=CARTESIAN_POINT('Ctrl Pts',(3.35214708226765,0.131295993814186,1.29795075602263));
#10751=CARTESIAN_POINT('Ctrl Pts',(3.35419203896924,0.143986470216691,1.31647293736623));
#10752=CARTESIAN_POINT('Ctrl Pts',(3.35708792761402,0.160839719007584,1.35711110492666));
#10753=CARTESIAN_POINT('Ctrl Pts',(3.35789496093577,0.165,1.37923124059256));
#10754=CARTESIAN_POINT('Ctrl Pts',(3.35789496093577,0.165,1.4));
#10755=CARTESIAN_POINT('Ctrl Pts',(3.34264068711929,2.77555756156289E-17,
1.565));
#10756=CARTESIAN_POINT('Ctrl Pts',(3.34264068711929,-0.0207679427235068,
1.565));
#10757=CARTESIAN_POINT('Ctrl Pts',(3.3434324152587,-0.0428883760934127,
1.56083992183864));
#10758=CARTESIAN_POINT('Ctrl Pts',(3.34629359821974,-0.0835273920906823,
1.54398634598358));
#10759=CARTESIAN_POINT('Ctrl Pts',(3.34832345279534,-0.102049819008125,
1.53129541878344));
#10760=CARTESIAN_POINT('Ctrl Pts',(3.35214708226765,-0.131295993814186,
1.50204924397737));
#10761=CARTESIAN_POINT('Ctrl Pts',(3.35419203896924,-0.143986470216691,
1.48352706263377));
#10762=CARTESIAN_POINT('Ctrl Pts',(3.35708792761402,-0.160839719007584,
1.44288889507334));
#10763=CARTESIAN_POINT('Ctrl Pts',(3.35789496093577,-0.165,1.42076875940744));
#10764=CARTESIAN_POINT('Ctrl Pts',(3.35789496093577,-0.165,1.37923124059256));
#10765=CARTESIAN_POINT('Ctrl Pts',(3.35708792761402,-0.160839719007584,
1.35711110492666));
#10766=CARTESIAN_POINT('Ctrl Pts',(3.35419203896924,-0.143986470216691,
1.31647293736623));
#10767=CARTESIAN_POINT('Ctrl Pts',(3.35214708226765,-0.131295993814186,
1.29795075602263));
#10768=CARTESIAN_POINT('Ctrl Pts',(3.34832345279534,-0.102049819008125,
1.26870458121656));
#10769=CARTESIAN_POINT('Ctrl Pts',(3.34629359821974,-0.0835273920906824,
1.25601365401642));
#10770=CARTESIAN_POINT('Ctrl Pts',(3.3434324152587,-0.0428883760934128,
1.23916007816136));
#10771=CARTESIAN_POINT('Ctrl Pts',(3.34264068711929,-0.0207679427235068,
1.235));
#10772=CARTESIAN_POINT('Ctrl Pts',(3.34264068711929,-4.16333634234434E-17,
1.235));
#10773=CARTESIAN_POINT('',(3.73764068711929,-1.70422299968729E-17,1.565));
#10774=CARTESIAN_POINT('',(3.24264069,-2.02066721859313E-17,1.565));
#10775=CARTESIAN_POINT('',(3.75264069,-0.122167928782887,1.51090535233657));
#10776=CARTESIAN_POINT('Ctrl Pts',(3.75264069,-0.122167928782887,1.51090535233657));
#10777=CARTESIAN_POINT('Ctrl Pts',(3.75219215735201,-0.120368921478644,
1.51288705106972));
#10778=CARTESIAN_POINT('Ctrl Pts',(3.75174544269427,-0.118534900551874,
1.51481033723969));
#10779=CARTESIAN_POINT('Ctrl Pts',(3.74784567158764,-0.102111993019358,
1.5312332447722));
#10780=CARTESIAN_POINT('Ctrl Pts',(3.74419817251169,-0.0836597150224319,
1.54390845611142));
#10781=CARTESIAN_POINT('Ctrl Pts',(3.73906286735823,-0.0430495960471595,
1.56079590960766));
#10782=CARTESIAN_POINT('Ctrl Pts',(3.73764068711929,-0.020880094330741,
1.565));
#10783=CARTESIAN_POINT('Ctrl Pts',(3.73764068711929,-2.08166817117217E-17,
1.565));
#10784=CARTESIAN_POINT('',(3.75264069,-0.122167928782887,1.28909464766343));
#10785=CARTESIAN_POINT('Origin',(3.75264069,0.,1.4));
#10786=CARTESIAN_POINT('',(3.73764068711929,-3.09223316784707E-17,1.235));
#10787=CARTESIAN_POINT('Ctrl Pts',(3.73764068711929,-1.38777878078145E-17,
1.235));
#10788=CARTESIAN_POINT('Ctrl Pts',(3.73764068711929,-0.020880094330741,
1.235));
#10789=CARTESIAN_POINT('Ctrl Pts',(3.73906286735823,-0.0430495960471595,
1.23920409039234));
#10790=CARTESIAN_POINT('Ctrl Pts',(3.74419817251169,-0.0836597150224319,
1.25609154388858));
#10791=CARTESIAN_POINT('Ctrl Pts',(3.74784567158764,-0.102111993019358,
1.2687667552278));
#10792=CARTESIAN_POINT('Ctrl Pts',(3.75174544269427,-0.118534900551874,
1.28518966276031));
#10793=CARTESIAN_POINT('Ctrl Pts',(3.75219215735201,-0.120368921478644,
1.28711294893028));
#10794=CARTESIAN_POINT('Ctrl Pts',(3.75264069,-0.122167928782887,1.28909464766343));
#10795=CARTESIAN_POINT('Ctrl Pts',(3.75264069,0.122167928782887,1.28909464766343));
#10796=CARTESIAN_POINT('Ctrl Pts',(3.75219215735201,0.120368921478644,1.28711294893028));
#10797=CARTESIAN_POINT('Ctrl Pts',(3.75174544269427,0.118534900551874,1.28518966276031));
#10798=CARTESIAN_POINT('Ctrl Pts',(3.74784567158764,0.102111993019358,1.2687667552278));
#10799=CARTESIAN_POINT('Ctrl Pts',(3.74419817251169,0.0836597150224319,
1.25609154388858));
#10800=CARTESIAN_POINT('Ctrl Pts',(3.73906286735823,0.0430495960471595,
1.23920409039234));
#10801=CARTESIAN_POINT('Ctrl Pts',(3.73764068711929,0.020880094330741,1.235));
#10802=CARTESIAN_POINT('Ctrl Pts',(3.73764068711929,0.,1.235));
#10803=CARTESIAN_POINT('Ctrl Pts',(3.73764068711929,-6.93889390390723E-18,
1.565));
#10804=CARTESIAN_POINT('Ctrl Pts',(3.73764068711929,0.020880094330741,1.565));
#10805=CARTESIAN_POINT('Ctrl Pts',(3.73906286735823,0.0430495960471595,
1.56079590960766));
#10806=CARTESIAN_POINT('Ctrl Pts',(3.74419817251169,0.0836597150224318,
1.54390845611142));
#10807=CARTESIAN_POINT('Ctrl Pts',(3.74784567158764,0.102111993019358,1.5312332447722));
#10808=CARTESIAN_POINT('Ctrl Pts',(3.75174544269427,0.118534900551874,1.51481033723969));
#10809=CARTESIAN_POINT('Ctrl Pts',(3.75219215735201,0.120368921478644,1.51288705106972));
#10810=CARTESIAN_POINT('Ctrl Pts',(3.75264069,0.122167928782887,1.51090535233657));
#10811=CARTESIAN_POINT('Origin',(3.75264069,0.,1.4));
#10812=CARTESIAN_POINT('',(3.75264069,-0.122167928782887,1.));
#10813=CARTESIAN_POINT('Origin',(4.24264068711929,0.,1.));
#10814=CARTESIAN_POINT('',(3.73764068711929,-6.18446633569413E-17,1.8));
#10815=CARTESIAN_POINT('Origin',(4.24264068711929,0.,1.8));
#10816=CARTESIAN_POINT('',(3.73764068711929,-6.18446633569413E-17,1.));
#10817=CARTESIAN_POINT('',(3.73764068711929,-6.18446633569413E-17,1.));
#10818=CARTESIAN_POINT('',(3.73764068711929,-6.18446633569413E-17,1.));
#10819=CARTESIAN_POINT('Origin',(4.24264068711929,0.,1.));
#10820=CARTESIAN_POINT('Origin',(4.24264068711929,0.,1.));
#10821=CARTESIAN_POINT('',(3.34264068711929,-1.10218211923262E-16,1.8));
#10822=CARTESIAN_POINT('Origin',(4.24264068711929,0.,1.8));
#10823=CARTESIAN_POINT('',(3.34264068711929,-1.10218211923262E-16,1.));
#10824=CARTESIAN_POINT('',(3.34264068711929,-1.10218211923262E-16,1.));
#10825=CARTESIAN_POINT('',(3.34264068711929,-1.10218211923262E-16,1.));
#10826=CARTESIAN_POINT('Origin',(4.24264068711929,0.,1.));
#10827=CARTESIAN_POINT('Origin',(4.24264068711929,0.,1.8));
#10828=CARTESIAN_POINT('Origin',(4.24264068711929,0.,1.));
#10829=CARTESIAN_POINT('',(0.,0.,0.));
#10830=CARTESIAN_POINT('Origin',(0.,-0.4,0.));
#10831=CARTESIAN_POINT('',(-0.1954,-0.4,2.39295984553393E-17));
#10832=CARTESIAN_POINT('Origin',(0.,-0.4,0.));
#10833=CARTESIAN_POINT('Origin',(0.0577350269189626,0.,-0.1));
#10834=CARTESIAN_POINT('',(0.0577350269189626,0.,-0.1));
#10835=CARTESIAN_POINT('',(0.115470053837925,0.,0.));
#10836=CARTESIAN_POINT('',(0.0934187836487032,0.,-0.0381939203391614));
#10837=CARTESIAN_POINT('',(0.0577350269189626,-0.2,-0.1));
#10838=CARTESIAN_POINT('',(0.0577350269189626,0.,-0.1));
#10839=CARTESIAN_POINT('',(0.115470053837925,-0.2,0.));
#10840=CARTESIAN_POINT('',(0.115470053837925,-0.2,0.));
#10841=CARTESIAN_POINT('',(0.115470053837925,0.,0.));
#10842=CARTESIAN_POINT('Origin',(-0.0577350269189626,0.,-0.1));
#10843=CARTESIAN_POINT('',(-0.0577350269189626,0.,-0.1));
#10844=CARTESIAN_POINT('',(0.0561324865405187,0.,-0.1));
#10845=CARTESIAN_POINT('',(-0.0577350269189626,-0.2,-0.1));
#10846=CARTESIAN_POINT('',(-0.0577350269189626,0.,-0.1));
#10847=CARTESIAN_POINT('',(0.0577350269189626,-0.2,-0.1));
#10848=CARTESIAN_POINT('Origin',(-0.115470053837925,0.,-1.38777878078145E-17));
#10849=CARTESIAN_POINT('',(-0.115470053837925,0.,-1.41410031829988E-17));
#10850=CARTESIAN_POINT('',(-0.0797862971081845,0.,-0.0618060796608387));
#10851=CARTESIAN_POINT('',(-0.115470053837925,-0.2,-1.38777878078145E-17));
#10852=CARTESIAN_POINT('',(-0.115470053837925,0.,-1.41410031829988E-17));
#10853=CARTESIAN_POINT('',(-0.0577350269189626,-0.2,-0.1));
#10854=CARTESIAN_POINT('Origin',(-0.0577350269189626,0.,0.1));
#10855=CARTESIAN_POINT('',(-0.0577350269189626,0.,0.1));
#10856=CARTESIAN_POINT('',(-0.0509187836487033,0.,0.111806079660839));
#10857=CARTESIAN_POINT('',(-0.0577350269189626,-0.2,0.1));
#10858=CARTESIAN_POINT('',(-0.0577350269189626,0.,0.1));
#10859=CARTESIAN_POINT('',(-0.115470053837925,-0.2,-1.41410031829988E-17));
#10860=CARTESIAN_POINT('Origin',(0.0577350269189626,0.,0.1));
#10861=CARTESIAN_POINT('',(0.0577350269189626,0.,0.1));
#10862=CARTESIAN_POINT('',(0.113867513459481,0.,0.1));
#10863=CARTESIAN_POINT('',(0.0577350269189626,-0.2,0.1));
#10864=CARTESIAN_POINT('',(0.0577350269189626,0.,0.1));
#10865=CARTESIAN_POINT('',(-0.0577350269189626,-0.2,0.1));
#10866=CARTESIAN_POINT('Origin',(0.115470053837925,0.,0.));
#10867=CARTESIAN_POINT('',(0.122286297108185,0.,-0.0118060796608386));
#10868=CARTESIAN_POINT('',(0.0577350269189626,-0.2,0.1));
#10869=CARTESIAN_POINT('Origin',(0.,-0.2,0.));
#10870=CARTESIAN_POINT('Origin',(0.17,0.,0.));
#10871=CARTESIAN_POINT('',(-0.17,-8.67361737988404E-18,-2.0818995585505E-17));
#10872=CARTESIAN_POINT('Origin',(0.,0.,0.));
#10873=CARTESIAN_POINT('Origin',(0.,-0.015,0.));
#10874=CARTESIAN_POINT('',(-0.1954,-0.0254,-2.39295984553393E-17));
#10875=CARTESIAN_POINT('Origin',(0.,-0.0254,0.));
#10876=CARTESIAN_POINT('',(-0.185,-0.015,-2.2655965784226E-17));
#10877=CARTESIAN_POINT('Origin',(0.,-0.2775,0.));
#10878=CARTESIAN_POINT('',(-0.1954,-0.2775,-2.39295984553393E-17));
#10879=CARTESIAN_POINT('',(0.,0.,0.));
#10880=CARTESIAN_POINT('',(0.,0.,0.));
#10881=CARTESIAN_POINT('',(0.,0.,0.));
#10882=CARTESIAN_POINT('',(0.,0.,0.));
#10883=CARTESIAN_POINT('',(0.,0.,0.));
#10884=CARTESIAN_POINT('',(0.,0.,0.));
#10885=CARTESIAN_POINT('',(0.,0.,0.));
#10886=CARTESIAN_POINT('',(0.,0.,0.));
#10887=CARTESIAN_POINT('',(0.,-0.9,1.4));
#10888=CARTESIAN_POINT('',(0.,0.,7.));
#10889=CARTESIAN_POINT('',(0.,0.,0.));
#10890=CARTESIAN_POINT('',(0.,0.,0.));
#10891=CARTESIAN_POINT('',(0.,0.,0.));
#10892=CARTESIAN_POINT('',(4.24264068711929,-0.9,1.4));
#10893=CARTESIAN_POINT('',(0.,0.,0.));
#10894=CARTESIAN_POINT('',(0.,0.,0.));
#10895=CARTESIAN_POINT('',(0.,0.,0.));
#10896=UNCERTAINTY_MEASURE_WITH_UNIT(LENGTH_MEASURE(0.001),#10958,
'DISTANCE_ACCURACY_VALUE',
'Maximum model space distance between geometric entities at asserted c
onnectivities');
#10897=UNCERTAINTY_MEASURE_WITH_UNIT(LENGTH_MEASURE(0.001),#10958,
'DISTANCE_ACCURACY_VALUE',
'Maximum model space distance between geometric entities at asserted c
onnectivities');
#10898=UNCERTAINTY_MEASURE_WITH_UNIT(LENGTH_MEASURE(0.001),#10958,
'DISTANCE_ACCURACY_VALUE',
'Maximum model space distance between geometric entities at asserted c
onnectivities');
#10899=UNCERTAINTY_MEASURE_WITH_UNIT(LENGTH_MEASURE(0.001),#10958,
'DISTANCE_ACCURACY_VALUE',
'Maximum model space distance between geometric entities at asserted c
onnectivities');
#10900=UNCERTAINTY_MEASURE_WITH_UNIT(LENGTH_MEASURE(0.001),#10958,
'DISTANCE_ACCURACY_VALUE',
'Maximum model space distance between geometric entities at asserted c
onnectivities');
#10901=UNCERTAINTY_MEASURE_WITH_UNIT(LENGTH_MEASURE(0.001),#10958,
'DISTANCE_ACCURACY_VALUE',
'Maximum model space distance between geometric entities at asserted c
onnectivities');
#10902=UNCERTAINTY_MEASURE_WITH_UNIT(LENGTH_MEASURE(0.001),#10958,
'DISTANCE_ACCURACY_VALUE',
'Maximum model space distance between geometric entities at asserted c
onnectivities');
#10903=UNCERTAINTY_MEASURE_WITH_UNIT(LENGTH_MEASURE(0.001),#10958,
'DISTANCE_ACCURACY_VALUE',
'Maximum model space distance between geometric entities at asserted c
onnectivities');
#10904=UNCERTAINTY_MEASURE_WITH_UNIT(LENGTH_MEASURE(0.001),#10958,
'DISTANCE_ACCURACY_VALUE',
'Maximum model space distance between geometric entities at asserted c
onnectivities');
#10905=UNCERTAINTY_MEASURE_WITH_UNIT(LENGTH_MEASURE(0.001),#10958,
'DISTANCE_ACCURACY_VALUE',
'Maximum model space distance between geometric entities at asserted c
onnectivities');
#10906=UNCERTAINTY_MEASURE_WITH_UNIT(LENGTH_MEASURE(0.001),#10958,
'DISTANCE_ACCURACY_VALUE',
'Maximum model space distance between geometric entities at asserted c
onnectivities');
#10907=UNCERTAINTY_MEASURE_WITH_UNIT(LENGTH_MEASURE(0.001),#10958,
'DISTANCE_ACCURACY_VALUE',
'Maximum model space distance between geometric entities at asserted c
onnectivities');
#10908=UNCERTAINTY_MEASURE_WITH_UNIT(LENGTH_MEASURE(0.001),#10958,
'DISTANCE_ACCURACY_VALUE',
'Maximum model space distance between geometric entities at asserted c
onnectivities');
#10909=UNCERTAINTY_MEASURE_WITH_UNIT(LENGTH_MEASURE(0.001),#10958,
'DISTANCE_ACCURACY_VALUE',
'Maximum model space distance between geometric entities at asserted c
onnectivities');
#10910=UNCERTAINTY_MEASURE_WITH_UNIT(LENGTH_MEASURE(0.001),#10958,
'DISTANCE_ACCURACY_VALUE',
'Maximum model space distance between geometric entities at asserted c
onnectivities');
#10911=UNCERTAINTY_MEASURE_WITH_UNIT(LENGTH_MEASURE(0.001),#10958,
'DISTANCE_ACCURACY_VALUE',
'Maximum model space distance between geometric entities at asserted c
onnectivities');
#10912=UNCERTAINTY_MEASURE_WITH_UNIT(LENGTH_MEASURE(0.001),#10958,
'DISTANCE_ACCURACY_VALUE',
'Maximum model space distance between geometric entities at asserted c
onnectivities');
#10913=UNCERTAINTY_MEASURE_WITH_UNIT(LENGTH_MEASURE(0.001),#10958,
'DISTANCE_ACCURACY_VALUE',
'Maximum model space distance between geometric entities at asserted c
onnectivities');
#10914=UNCERTAINTY_MEASURE_WITH_UNIT(LENGTH_MEASURE(0.001),#10958,
'DISTANCE_ACCURACY_VALUE',
'Maximum model space distance between geometric entities at asserted c
onnectivities');
#10915=UNCERTAINTY_MEASURE_WITH_UNIT(LENGTH_MEASURE(0.001),#10958,
'DISTANCE_ACCURACY_VALUE',
'Maximum model space distance between geometric entities at asserted c
onnectivities');
#10916=UNCERTAINTY_MEASURE_WITH_UNIT(LENGTH_MEASURE(0.001),#10958,
'DISTANCE_ACCURACY_VALUE',
'Maximum model space distance between geometric entities at asserted c
onnectivities');
#10917=UNCERTAINTY_MEASURE_WITH_UNIT(LENGTH_MEASURE(0.001),#10958,
'DISTANCE_ACCURACY_VALUE',
'Maximum model space distance between geometric entities at asserted c
onnectivities');
#10918=UNCERTAINTY_MEASURE_WITH_UNIT(LENGTH_MEASURE(0.001),#10958,
'DISTANCE_ACCURACY_VALUE',
'Maximum model space distance between geometric entities at asserted c
onnectivities');
#10919=UNCERTAINTY_MEASURE_WITH_UNIT(LENGTH_MEASURE(0.001),#10958,
'DISTANCE_ACCURACY_VALUE',
'Maximum model space distance between geometric entities at asserted c
onnectivities');
#10920=UNCERTAINTY_MEASURE_WITH_UNIT(LENGTH_MEASURE(0.001),#10958,
'DISTANCE_ACCURACY_VALUE',
'Maximum model space distance between geometric entities at asserted c
onnectivities');
#10921=UNCERTAINTY_MEASURE_WITH_UNIT(LENGTH_MEASURE(0.001),#10958,
'DISTANCE_ACCURACY_VALUE',
'Maximum model space distance between geometric entities at asserted c
onnectivities');
#10922=UNCERTAINTY_MEASURE_WITH_UNIT(LENGTH_MEASURE(0.001),#10958,
'DISTANCE_ACCURACY_VALUE',
'Maximum model space distance between geometric entities at asserted c
onnectivities');
#10923=UNCERTAINTY_MEASURE_WITH_UNIT(LENGTH_MEASURE(0.001),#10958,
'DISTANCE_ACCURACY_VALUE',
'Maximum model space distance between geometric entities at asserted c
onnectivities');
#10924=UNCERTAINTY_MEASURE_WITH_UNIT(LENGTH_MEASURE(0.001),#10958,
'DISTANCE_ACCURACY_VALUE',
'Maximum model space distance between geometric entities at asserted c
onnectivities');
#10925=UNCERTAINTY_MEASURE_WITH_UNIT(LENGTH_MEASURE(0.001),#10958,
'DISTANCE_ACCURACY_VALUE',
'Maximum model space distance between geometric entities at asserted c
onnectivities');
#10926=UNCERTAINTY_MEASURE_WITH_UNIT(LENGTH_MEASURE(0.001),#10958,
'DISTANCE_ACCURACY_VALUE',
'Maximum model space distance between geometric entities at asserted c
onnectivities');
#10927=(
GEOMETRIC_REPRESENTATION_CONTEXT(3)
GLOBAL_UNCERTAINTY_ASSIGNED_CONTEXT((#10896))
GLOBAL_UNIT_ASSIGNED_CONTEXT((#10958,#10960,#10961))
REPRESENTATION_CONTEXT('','3D')
);
#10928=(
GEOMETRIC_REPRESENTATION_CONTEXT(3)
GLOBAL_UNCERTAINTY_ASSIGNED_CONTEXT((#10897))
GLOBAL_UNIT_ASSIGNED_CONTEXT((#10958,#10960,#10961))
REPRESENTATION_CONTEXT('','3D')
);
#10929=(
GEOMETRIC_REPRESENTATION_CONTEXT(3)
GLOBAL_UNCERTAINTY_ASSIGNED_CONTEXT((#10898))
GLOBAL_UNIT_ASSIGNED_CONTEXT((#10958,#10960,#10961))
REPRESENTATION_CONTEXT('','3D')
);
#10930=(
GEOMETRIC_REPRESENTATION_CONTEXT(3)
GLOBAL_UNCERTAINTY_ASSIGNED_CONTEXT((#10899))
GLOBAL_UNIT_ASSIGNED_CONTEXT((#10958,#10960,#10961))
REPRESENTATION_CONTEXT('','3D')
);
#10931=(
GEOMETRIC_REPRESENTATION_CONTEXT(3)
GLOBAL_UNCERTAINTY_ASSIGNED_CONTEXT((#10900))
GLOBAL_UNIT_ASSIGNED_CONTEXT((#10958,#10960,#10961))
REPRESENTATION_CONTEXT('','3D')
);
#10932=(
GEOMETRIC_REPRESENTATION_CONTEXT(3)
GLOBAL_UNCERTAINTY_ASSIGNED_CONTEXT((#10901))
GLOBAL_UNIT_ASSIGNED_CONTEXT((#10958,#10960,#10961))
REPRESENTATION_CONTEXT('','3D')
);
#10933=(
GEOMETRIC_REPRESENTATION_CONTEXT(3)
GLOBAL_UNCERTAINTY_ASSIGNED_CONTEXT((#10902))
GLOBAL_UNIT_ASSIGNED_CONTEXT((#10958,#10960,#10961))
REPRESENTATION_CONTEXT('','3D')
);
#10934=(
GEOMETRIC_REPRESENTATION_CONTEXT(3)
GLOBAL_UNCERTAINTY_ASSIGNED_CONTEXT((#10903))
GLOBAL_UNIT_ASSIGNED_CONTEXT((#10958,#10960,#10961))
REPRESENTATION_CONTEXT('','3D')
);
#10935=(
GEOMETRIC_REPRESENTATION_CONTEXT(3)
GLOBAL_UNCERTAINTY_ASSIGNED_CONTEXT((#10904))
GLOBAL_UNIT_ASSIGNED_CONTEXT((#10958,#10960,#10961))
REPRESENTATION_CONTEXT('','3D')
);
#10936=(
GEOMETRIC_REPRESENTATION_CONTEXT(3)
GLOBAL_UNCERTAINTY_ASSIGNED_CONTEXT((#10905))
GLOBAL_UNIT_ASSIGNED_CONTEXT((#10958,#10960,#10961))
REPRESENTATION_CONTEXT('','3D')
);
#10937=(
GEOMETRIC_REPRESENTATION_CONTEXT(3)
GLOBAL_UNCERTAINTY_ASSIGNED_CONTEXT((#10906))
GLOBAL_UNIT_ASSIGNED_CONTEXT((#10958,#10960,#10961))
REPRESENTATION_CONTEXT('','3D')
);
#10938=(
GEOMETRIC_REPRESENTATION_CONTEXT(3)
GLOBAL_UNCERTAINTY_ASSIGNED_CONTEXT((#10907))
GLOBAL_UNIT_ASSIGNED_CONTEXT((#10958,#10960,#10961))
REPRESENTATION_CONTEXT('','3D')
);
#10939=(
GEOMETRIC_REPRESENTATION_CONTEXT(3)
GLOBAL_UNCERTAINTY_ASSIGNED_CONTEXT((#10908))
GLOBAL_UNIT_ASSIGNED_CONTEXT((#10958,#10960,#10961))
REPRESENTATION_CONTEXT('','3D')
);
#10940=(
GEOMETRIC_REPRESENTATION_CONTEXT(3)
GLOBAL_UNCERTAINTY_ASSIGNED_CONTEXT((#10909))
GLOBAL_UNIT_ASSIGNED_CONTEXT((#10958,#10960,#10961))
REPRESENTATION_CONTEXT('','3D')
);
#10941=(
GEOMETRIC_REPRESENTATION_CONTEXT(3)
GLOBAL_UNCERTAINTY_ASSIGNED_CONTEXT((#10910))
GLOBAL_UNIT_ASSIGNED_CONTEXT((#10958,#10960,#10961))
REPRESENTATION_CONTEXT('','3D')
);
#10942=(
GEOMETRIC_REPRESENTATION_CONTEXT(3)
GLOBAL_UNCERTAINTY_ASSIGNED_CONTEXT((#10911))
GLOBAL_UNIT_ASSIGNED_CONTEXT((#10958,#10960,#10961))
REPRESENTATION_CONTEXT('','3D')
);
#10943=(
GEOMETRIC_REPRESENTATION_CONTEXT(3)
GLOBAL_UNCERTAINTY_ASSIGNED_CONTEXT((#10912))
GLOBAL_UNIT_ASSIGNED_CONTEXT((#10958,#10960,#10961))
REPRESENTATION_CONTEXT('','3D')
);
#10944=(
GEOMETRIC_REPRESENTATION_CONTEXT(3)
GLOBAL_UNCERTAINTY_ASSIGNED_CONTEXT((#10913))
GLOBAL_UNIT_ASSIGNED_CONTEXT((#10958,#10960,#10961))
REPRESENTATION_CONTEXT('','3D')
);
#10945=(
GEOMETRIC_REPRESENTATION_CONTEXT(3)
GLOBAL_UNCERTAINTY_ASSIGNED_CONTEXT((#10914))
GLOBAL_UNIT_ASSIGNED_CONTEXT((#10958,#10960,#10961))
REPRESENTATION_CONTEXT('','3D')
);
#10946=(
GEOMETRIC_REPRESENTATION_CONTEXT(3)
GLOBAL_UNCERTAINTY_ASSIGNED_CONTEXT((#10915))
GLOBAL_UNIT_ASSIGNED_CONTEXT((#10958,#10960,#10961))
REPRESENTATION_CONTEXT('','3D')
);
#10947=(
GEOMETRIC_REPRESENTATION_CONTEXT(3)
GLOBAL_UNCERTAINTY_ASSIGNED_CONTEXT((#10916))
GLOBAL_UNIT_ASSIGNED_CONTEXT((#10958,#10960,#10961))
REPRESENTATION_CONTEXT('','3D')
);
#10948=(
GEOMETRIC_REPRESENTATION_CONTEXT(3)
GLOBAL_UNCERTAINTY_ASSIGNED_CONTEXT((#10917))
GLOBAL_UNIT_ASSIGNED_CONTEXT((#10958,#10960,#10961))
REPRESENTATION_CONTEXT('','3D')
);
#10949=(
GEOMETRIC_REPRESENTATION_CONTEXT(3)
GLOBAL_UNCERTAINTY_ASSIGNED_CONTEXT((#10918))
GLOBAL_UNIT_ASSIGNED_CONTEXT((#10958,#10960,#10961))
REPRESENTATION_CONTEXT('','3D')
);
#10950=(
GEOMETRIC_REPRESENTATION_CONTEXT(3)
GLOBAL_UNCERTAINTY_ASSIGNED_CONTEXT((#10919))
GLOBAL_UNIT_ASSIGNED_CONTEXT((#10958,#10960,#10961))
REPRESENTATION_CONTEXT('','3D')
);
#10951=(
GEOMETRIC_REPRESENTATION_CONTEXT(3)
GLOBAL_UNCERTAINTY_ASSIGNED_CONTEXT((#10920))
GLOBAL_UNIT_ASSIGNED_CONTEXT((#10958,#10960,#10961))
REPRESENTATION_CONTEXT('','3D')
);
#10952=(
GEOMETRIC_REPRESENTATION_CONTEXT(3)
GLOBAL_UNCERTAINTY_ASSIGNED_CONTEXT((#10921))
GLOBAL_UNIT_ASSIGNED_CONTEXT((#10958,#10960,#10961))
REPRESENTATION_CONTEXT('','3D')
);
#10953=(
GEOMETRIC_REPRESENTATION_CONTEXT(3)
GLOBAL_UNCERTAINTY_ASSIGNED_CONTEXT((#10922))
GLOBAL_UNIT_ASSIGNED_CONTEXT((#10958,#10960,#10961))
REPRESENTATION_CONTEXT('','3D')
);
#10954=(
GEOMETRIC_REPRESENTATION_CONTEXT(3)
GLOBAL_UNCERTAINTY_ASSIGNED_CONTEXT((#10923))
GLOBAL_UNIT_ASSIGNED_CONTEXT((#10958,#10960,#10961))
REPRESENTATION_CONTEXT('','3D')
);
#10955=(
GEOMETRIC_REPRESENTATION_CONTEXT(3)
GLOBAL_UNCERTAINTY_ASSIGNED_CONTEXT((#10924))
GLOBAL_UNIT_ASSIGNED_CONTEXT((#10958,#10960,#10961))
REPRESENTATION_CONTEXT('','3D')
);
#10956=(
GEOMETRIC_REPRESENTATION_CONTEXT(3)
GLOBAL_UNCERTAINTY_ASSIGNED_CONTEXT((#10925))
GLOBAL_UNIT_ASSIGNED_CONTEXT((#10958,#10960,#10961))
REPRESENTATION_CONTEXT('','3D')
);
#10957=(
GEOMETRIC_REPRESENTATION_CONTEXT(3)
GLOBAL_UNCERTAINTY_ASSIGNED_CONTEXT((#10926))
GLOBAL_UNIT_ASSIGNED_CONTEXT((#10958,#10960,#10961))
REPRESENTATION_CONTEXT('','3D')
);
#10958=(
LENGTH_UNIT()
NAMED_UNIT(*)
SI_UNIT(.CENTI.,.METRE.)
);
#10959=(
LENGTH_UNIT()
NAMED_UNIT(*)
SI_UNIT($,.METRE.)
);
#10960=(
NAMED_UNIT(*)
PLANE_ANGLE_UNIT()
SI_UNIT($,.RADIAN.)
);
#10961=(
NAMED_UNIT(*)
SI_UNIT($,.STERADIAN.)
SOLID_ANGLE_UNIT()
);
#10962=SHAPE_DEFINITION_REPRESENTATION(#10992,#11064);
#10963=SHAPE_DEFINITION_REPRESENTATION(#10993,#11065);
#10964=SHAPE_DEFINITION_REPRESENTATION(#10994,#11066);
#10965=SHAPE_DEFINITION_REPRESENTATION(#10995,#11067);
#10966=SHAPE_DEFINITION_REPRESENTATION(#10996,#11068);
#10967=SHAPE_DEFINITION_REPRESENTATION(#10997,#11069);
#10968=SHAPE_DEFINITION_REPRESENTATION(#10998,#11070);
#10969=SHAPE_DEFINITION_REPRESENTATION(#10999,#11071);
#10970=SHAPE_DEFINITION_REPRESENTATION(#11000,#11072);
#10971=SHAPE_DEFINITION_REPRESENTATION(#11001,#11073);
#10972=SHAPE_DEFINITION_REPRESENTATION(#11002,#11074);
#10973=SHAPE_DEFINITION_REPRESENTATION(#11003,#11075);
#10974=SHAPE_DEFINITION_REPRESENTATION(#11004,#11076);
#10975=SHAPE_DEFINITION_REPRESENTATION(#11005,#11077);
#10976=SHAPE_DEFINITION_REPRESENTATION(#11006,#11078);
#10977=SHAPE_DEFINITION_REPRESENTATION(#11012,#11079);
#10978=SHAPE_DEFINITION_REPRESENTATION(#11013,#11080);
#10979=SHAPE_DEFINITION_REPRESENTATION(#11014,#11081);
#10980=SHAPE_DEFINITION_REPRESENTATION(#11015,#11082);
#10981=SHAPE_DEFINITION_REPRESENTATION(#11016,#11083);
#10982=SHAPE_DEFINITION_REPRESENTATION(#11017,#11084);
#10983=SHAPE_DEFINITION_REPRESENTATION(#11018,#11085);
#10984=SHAPE_DEFINITION_REPRESENTATION(#11019,#11086);
#10985=SHAPE_DEFINITION_REPRESENTATION(#11020,#11087);
#10986=SHAPE_DEFINITION_REPRESENTATION(#11021,#11088);
#10987=SHAPE_DEFINITION_REPRESENTATION(#11042,#11089);
#10988=SHAPE_DEFINITION_REPRESENTATION(#11043,#11090);
#10989=SHAPE_DEFINITION_REPRESENTATION(#11044,#11091);
#10990=SHAPE_DEFINITION_REPRESENTATION(#11045,#11092);
#10991=SHAPE_DEFINITION_REPRESENTATION(#11046,#11093);
#10992=PRODUCT_DEFINITION_SHAPE('',$,#11095);
#10993=PRODUCT_DEFINITION_SHAPE('',$,#11096);
#10994=PRODUCT_DEFINITION_SHAPE('',$,#11097);
#10995=PRODUCT_DEFINITION_SHAPE('',$,#11098);
#10996=PRODUCT_DEFINITION_SHAPE('',$,#11099);
#10997=PRODUCT_DEFINITION_SHAPE('',$,#11100);
#10998=PRODUCT_DEFINITION_SHAPE('',$,#11101);
#10999=PRODUCT_DEFINITION_SHAPE('',$,#11102);
#11000=PRODUCT_DEFINITION_SHAPE('',$,#11103);
#11001=PRODUCT_DEFINITION_SHAPE('',$,#11104);
#11002=PRODUCT_DEFINITION_SHAPE('',$,#11105);
#11003=PRODUCT_DEFINITION_SHAPE('',$,#11106);
#11004=PRODUCT_DEFINITION_SHAPE('',$,#11107);
#11005=PRODUCT_DEFINITION_SHAPE('',$,#11108);
#11006=PRODUCT_DEFINITION_SHAPE('',$,#11109);
#11007=PRODUCT_DEFINITION_SHAPE($,$,#137);
#11008=PRODUCT_DEFINITION_SHAPE($,$,#138);
#11009=PRODUCT_DEFINITION_SHAPE($,$,#139);
#11010=PRODUCT_DEFINITION_SHAPE($,$,#140);
#11011=PRODUCT_DEFINITION_SHAPE($,$,#141);
#11012=PRODUCT_DEFINITION_SHAPE('',$,#11110);
#11013=PRODUCT_DEFINITION_SHAPE('',$,#11111);
#11014=PRODUCT_DEFINITION_SHAPE('',$,#11112);
#11015=PRODUCT_DEFINITION_SHAPE('',$,#11113);
#11016=PRODUCT_DEFINITION_SHAPE('',$,#11114);
#11017=PRODUCT_DEFINITION_SHAPE('',$,#11115);
#11018=PRODUCT_DEFINITION_SHAPE('',$,#11116);
#11019=PRODUCT_DEFINITION_SHAPE('',$,#11117);
#11020=PRODUCT_DEFINITION_SHAPE('',$,#11118);
#11021=PRODUCT_DEFINITION_SHAPE('',$,#11119);
#11022=PRODUCT_DEFINITION_SHAPE($,$,#142);
#11023=PRODUCT_DEFINITION_SHAPE($,$,#143);
#11024=PRODUCT_DEFINITION_SHAPE($,$,#144);
#11025=PRODUCT_DEFINITION_SHAPE($,$,#145);
#11026=PRODUCT_DEFINITION_SHAPE($,$,#146);
#11027=PRODUCT_DEFINITION_SHAPE($,$,#147);
#11028=PRODUCT_DEFINITION_SHAPE($,$,#148);
#11029=PRODUCT_DEFINITION_SHAPE($,$,#149);
#11030=PRODUCT_DEFINITION_SHAPE($,$,#150);
#11031=PRODUCT_DEFINITION_SHAPE($,$,#151);
#11032=PRODUCT_DEFINITION_SHAPE($,$,#152);
#11033=PRODUCT_DEFINITION_SHAPE($,$,#153);
#11034=PRODUCT_DEFINITION_SHAPE($,$,#154);
#11035=PRODUCT_DEFINITION_SHAPE($,$,#155);
#11036=PRODUCT_DEFINITION_SHAPE($,$,#156);
#11037=PRODUCT_DEFINITION_SHAPE($,$,#157);
#11038=PRODUCT_DEFINITION_SHAPE($,$,#158);
#11039=PRODUCT_DEFINITION_SHAPE($,$,#159);
#11040=PRODUCT_DEFINITION_SHAPE($,$,#160);
#11041=PRODUCT_DEFINITION_SHAPE($,$,#161);
#11042=PRODUCT_DEFINITION_SHAPE('',$,#11120);
#11043=PRODUCT_DEFINITION_SHAPE('',$,#11121);
#11044=PRODUCT_DEFINITION_SHAPE('',$,#11122);
#11045=PRODUCT_DEFINITION_SHAPE('',$,#11123);
#11046=PRODUCT_DEFINITION_SHAPE('',$,#11124);
#11047=PRODUCT_DEFINITION_SHAPE($,$,#162);
#11048=PRODUCT_DEFINITION_SHAPE($,$,#163);
#11049=PRODUCT_DEFINITION_SHAPE($,$,#164);
#11050=PRODUCT_DEFINITION_SHAPE($,$,#165);
#11051=PRODUCT_DEFINITION_SHAPE($,$,#166);
#11052=PRODUCT_DEFINITION_SHAPE($,$,#167);
#11053=PRODUCT_DEFINITION_SHAPE($,$,#168);
#11054=PRODUCT_DEFINITION_SHAPE($,$,#169);
#11055=PRODUCT_DEFINITION_SHAPE($,$,#170);
#11056=PRODUCT_DEFINITION_SHAPE($,$,#171);
#11057=PRODUCT_DEFINITION_SHAPE($,$,#172);
#11058=PRODUCT_DEFINITION_SHAPE($,$,#173);
#11059=PRODUCT_DEFINITION_SHAPE($,$,#174);
#11060=PRODUCT_DEFINITION_SHAPE($,$,#175);
#11061=PRODUCT_DEFINITION_SHAPE($,$,#176);
#11062=PRODUCT_DEFINITION_SHAPE($,$,#177);
#11063=PRODUCT_DEFINITION_SHAPE($,$,#178);
#11064=SHAPE_REPRESENTATION('',(#6010,#6746,#6747,#6748),#10927);
#11065=SHAPE_REPRESENTATION('',(#6011,#6549,#6550,#6551,#6552,#6553,#6554,
#6555,#6556,#6557,#6558,#6559,#6560,#6561,#6562,#6563,#6564,#6565,#6566,
#6567,#6568),#10928);
#11066=SHAPE_REPRESENTATION('',(#6012),#10929);
#11067=SHAPE_REPRESENTATION('',(#6031),#10930);
#11068=SHAPE_REPRESENTATION('',(#6038),#10931);
#11069=SHAPE_REPRESENTATION('',(#6045),#10932);
#11070=SHAPE_REPRESENTATION('',(#6146),#10933);
#11071=SHAPE_REPRESENTATION('',(#6195),#10934);
#11072=SHAPE_REPRESENTATION('',(#6244),#10935);
#11073=SHAPE_REPRESENTATION('',(#6270,#6399,#6400,#6401,#6402,#6403),#10936);
#11074=SHAPE_REPRESENTATION('',(#6271),#10937);
#11075=SHAPE_REPRESENTATION('',(#6291),#10938);
#11076=SHAPE_REPRESENTATION('',(#6311),#10939);
#11077=SHAPE_REPRESENTATION('',(#6328),#10940);
#11078=SHAPE_REPRESENTATION('',(#6382),#10941);
#11079=SHAPE_REPRESENTATION('',(#6404,#6732,#6733,#6734,#6735,#6736,#6737,
#6738,#6739,#6740,#6741),#10942);
#11080=SHAPE_REPRESENTATION('',(#6405),#10943);
#11081=SHAPE_REPRESENTATION('',(#6441),#10944);
#11082=SHAPE_REPRESENTATION('',(#6450),#10945);
#11083=SHAPE_REPRESENTATION('',(#6470),#10946);
#11084=SHAPE_REPRESENTATION('',(#6484),#10947);
#11085=SHAPE_REPRESENTATION('',(#6498),#10948);
#11086=SHAPE_REPRESENTATION('',(#6507),#10949);
#11087=SHAPE_REPRESENTATION('',(#6516),#10950);
#11088=SHAPE_REPRESENTATION('',(#6525),#10951);
#11089=SHAPE_REPRESENTATION('',(#6569,#6742,#6743,#6744,#6745),#10952);
#11090=SHAPE_REPRESENTATION('',(#6570),#10953);
#11091=SHAPE_REPRESENTATION('',(#6688),#10954);
#11092=SHAPE_REPRESENTATION('',(#6697),#10955);
#11093=SHAPE_REPRESENTATION('',(#6717),#10956);
#11094=PRODUCT_DEFINITION_CONTEXT('part definition',#11186,'design');
#11095=PRODUCT_DEFINITION('PAT-021',
'PAT-021',#11125,#11094);
#11096=PRODUCT_DEFINITION('Bearing base','Bearing base',#11126,#11094);
#11097=PRODUCT_DEFINITION('Base','Base',#11127,#11094);
#11098=PRODUCT_DEFINITION('Foot strip','Foot strip',#11128,#11094);
#11099=PRODUCT_DEFINITION('Foot strip (1)','Foot strip (1)',#11129,#11094);
#11100=PRODUCT_DEFINITION('Twin bearing block','Twin bearing block',#11130,
#11094);
#11101=PRODUCT_DEFINITION('Bearing cap','Bearing cap',#11131,#11094);
#11102=PRODUCT_DEFINITION('Bearing cap (1)','Bearing cap (1)',#11132,#11094);
#11103=PRODUCT_DEFINITION('Cap Screw - M5x20','Cap Screw - M5x20',#11133,
#11094);
#11104=PRODUCT_DEFINITION('Sealed Ball Bearing - 10 x 30 x 9 mm',
'Sealed Ball Bearing - 10 x 30 x 9 mm',#11134,#11094);
#11105=PRODUCT_DEFINITION('Inner ring','Inner ring',#11135,#11094);
#11106=PRODUCT_DEFINITION('Outer ring','Outer ring',#11136,#11094);
#11107=PRODUCT_DEFINITION('Balls','Balls',#11137,#11094);
#11108=PRODUCT_DEFINITION('Cage','Cage',#11138,#11094);
#11109=PRODUCT_DEFINITION('Seals 2RS','Seals 2RS',#11139,#11094);
#11110=PRODUCT_DEFINITION('Input crank and locking cam',
'Input crank and locking cam',#11140,#11094);
#11111=PRODUCT_DEFINITION('Input crank and spindle',
'Input crank and spindle',#11141,#11094);
#11112=PRODUCT_DEFINITION('Lower bearing sleeve','Lower bearing sleeve',
#11142,#11094);
#11113=PRODUCT_DEFINITION('Retaining collar','Retaining collar',#11143,
#11094);
#11114=PRODUCT_DEFINITION('Drive pin','Drive pin',#11144,#11094);
#11115=PRODUCT_DEFINITION('Locking cam','Locking cam',#11145,#11094);
#11116=PRODUCT_DEFINITION('Locking cam spacer','Locking cam spacer',#11146,
#11094);
#11117=PRODUCT_DEFINITION('Cam keeper','Cam keeper',#11147,#11094);
#11118=PRODUCT_DEFINITION('Crank grip','Crank grip',#11148,#11094);
#11119=PRODUCT_DEFINITION('M4x10 Cap Screw','M4x10 Cap Screw',#11149,#11094);
#11120=PRODUCT_DEFINITION('Four-slot output wheel',
'Four-slot output wheel',#11150,#11094);
#11121=PRODUCT_DEFINITION('Output wheel and spindle',
'Output wheel and spindle',#11151,#11094);
#11122=PRODUCT_DEFINITION('Lower bearing sleeve (1)',
'Lower bearing sleeve (1)',#11152,#11094);
#11123=PRODUCT_DEFINITION('Retaining collar (1)','Retaining collar (1)',#11153,
#11094);
#11124=PRODUCT_DEFINITION('M4x4 collar screw','M4x4 collar screw',#11154,
#11094);
#11125=PRODUCT_DEFINITION_FORMATION('',$,#11188);
#11126=PRODUCT_DEFINITION_FORMATION('',$,#11189);
#11127=PRODUCT_DEFINITION_FORMATION('',$,#11190);
#11128=PRODUCT_DEFINITION_FORMATION('',$,#11191);
#11129=PRODUCT_DEFINITION_FORMATION('',$,#11192);
#11130=PRODUCT_DEFINITION_FORMATION('',$,#11193);
#11131=PRODUCT_DEFINITION_FORMATION('',$,#11194);
#11132=PRODUCT_DEFINITION_FORMATION('',$,#11195);
#11133=PRODUCT_DEFINITION_FORMATION('',$,#11196);
#11134=PRODUCT_DEFINITION_FORMATION('',$,#11197);
#11135=PRODUCT_DEFINITION_FORMATION('',$,#11198);
#11136=PRODUCT_DEFINITION_FORMATION('',$,#11199);
#11137=PRODUCT_DEFINITION_FORMATION('',$,#11200);
#11138=PRODUCT_DEFINITION_FORMATION('',$,#11201);
#11139=PRODUCT_DEFINITION_FORMATION('',$,#11202);
#11140=PRODUCT_DEFINITION_FORMATION('',$,#11203);
#11141=PRODUCT_DEFINITION_FORMATION('',$,#11204);
#11142=PRODUCT_DEFINITION_FORMATION('',$,#11205);
#11143=PRODUCT_DEFINITION_FORMATION('',$,#11206);
#11144=PRODUCT_DEFINITION_FORMATION('',$,#11207);
#11145=PRODUCT_DEFINITION_FORMATION('',$,#11208);
#11146=PRODUCT_DEFINITION_FORMATION('',$,#11209);
#11147=PRODUCT_DEFINITION_FORMATION('',$,#11210);
#11148=PRODUCT_DEFINITION_FORMATION('',$,#11211);
#11149=PRODUCT_DEFINITION_FORMATION('',$,#11212);
#11150=PRODUCT_DEFINITION_FORMATION('',$,#11213);
#11151=PRODUCT_DEFINITION_FORMATION('',$,#11214);
#11152=PRODUCT_DEFINITION_FORMATION('',$,#11215);
#11153=PRODUCT_DEFINITION_FORMATION('',$,#11216);
#11154=PRODUCT_DEFINITION_FORMATION('',$,#11217);
#11155=PRODUCT_RELATED_PRODUCT_CATEGORY('PAT-021','PAT-021',(#11188));
#11156=PRODUCT_RELATED_PRODUCT_CATEGORY('Bearing base','Bearing base',(#11189));
#11157=PRODUCT_RELATED_PRODUCT_CATEGORY('Base','Base',(#11190));
#11158=PRODUCT_RELATED_PRODUCT_CATEGORY('Foot strip','Foot strip',(#11191));
#11159=PRODUCT_RELATED_PRODUCT_CATEGORY('Foot strip (1)',
'Foot strip (1)',(#11192));
#11160=PRODUCT_RELATED_PRODUCT_CATEGORY('Twin bearing block',
'Twin bearing block',(#11193));
#11161=PRODUCT_RELATED_PRODUCT_CATEGORY('Bearing cap','Bearing cap',(#11194));
#11162=PRODUCT_RELATED_PRODUCT_CATEGORY('Bearing cap (1)',
'Bearing cap (1)',(#11195));
#11163=PRODUCT_RELATED_PRODUCT_CATEGORY('Cap Screw - M5x20',
'Cap Screw - M5x20',(#11196));
#11164=PRODUCT_RELATED_PRODUCT_CATEGORY(
'Sealed Ball Bearing - 10 x 30 x 9 mm',
'Sealed Ball Bearing - 10 x 30 x 9 mm',(#11197));
#11165=PRODUCT_RELATED_PRODUCT_CATEGORY('Inner ring','Inner ring',(#11198));
#11166=PRODUCT_RELATED_PRODUCT_CATEGORY('Outer ring','Outer ring',(#11199));
#11167=PRODUCT_RELATED_PRODUCT_CATEGORY('Balls','Balls',(#11200));
#11168=PRODUCT_RELATED_PRODUCT_CATEGORY('Cage','Cage',(#11201));
#11169=PRODUCT_RELATED_PRODUCT_CATEGORY('Seals 2RS','Seals 2RS',(#11202));
#11170=PRODUCT_RELATED_PRODUCT_CATEGORY('Input crank and locking cam',
'Input crank and locking cam',(#11203));
#11171=PRODUCT_RELATED_PRODUCT_CATEGORY('Input crank and spindle',
'Input crank and spindle',(#11204));
#11172=PRODUCT_RELATED_PRODUCT_CATEGORY('Lower bearing sleeve',
'Lower bearing sleeve',(#11205));
#11173=PRODUCT_RELATED_PRODUCT_CATEGORY('Retaining collar',
'Retaining collar',(#11206));
#11174=PRODUCT_RELATED_PRODUCT_CATEGORY('Drive pin','Drive pin',(#11207));
#11175=PRODUCT_RELATED_PRODUCT_CATEGORY('Locking cam','Locking cam',(#11208));
#11176=PRODUCT_RELATED_PRODUCT_CATEGORY('Locking cam spacer',
'Locking cam spacer',(#11209));
#11177=PRODUCT_RELATED_PRODUCT_CATEGORY('Cam keeper','Cam keeper',(#11210));
#11178=PRODUCT_RELATED_PRODUCT_CATEGORY('Crank grip','Crank grip',(#11211));
#11179=PRODUCT_RELATED_PRODUCT_CATEGORY('M4x10 Cap Screw',
'M4x10 Cap Screw',(#11212));
#11180=PRODUCT_RELATED_PRODUCT_CATEGORY('Four-slot output wheel',
'Four-slot output wheel',(#11213));
#11181=PRODUCT_RELATED_PRODUCT_CATEGORY('Output wheel and spindle',
'Output wheel and spindle',(#11214));
#11182=PRODUCT_RELATED_PRODUCT_CATEGORY('Lower bearing sleeve (1)',
'Lower bearing sleeve (1)',(#11215));
#11183=PRODUCT_RELATED_PRODUCT_CATEGORY('Retaining collar (1)',
'Retaining collar (1)',(#11216));
#11184=PRODUCT_RELATED_PRODUCT_CATEGORY('M4x4 collar screw',
'M4x4 collar screw',(#11217));
#11185=APPLICATION_PROTOCOL_DEFINITION('international standard',
'automotive_design',2009,#11186);
#11186=APPLICATION_CONTEXT(
'Core Data for Automotive Mechanical Design Process');
#11187=PRODUCT_CONTEXT('part definition',#11186,'mechanical');
#11188=PRODUCT('PAT-021','PAT-021',
'PAT-021',(#11187));
#11189=PRODUCT('Bearing base','Bearing base','Bearing base',(#11187));
#11190=PRODUCT('Base','Base','Base',(#11187));
#11191=PRODUCT('Foot strip','Foot strip','Foot strip',(#11187));
#11192=PRODUCT('Foot strip (1)','Foot strip (1)','Foot strip (1)',(#11187));
#11193=PRODUCT('Twin bearing block','Twin bearing block',
'Twin bearing block',(#11187));
#11194=PRODUCT('Bearing cap','Bearing cap','Bearing cap',(#11187));
#11195=PRODUCT('Bearing cap (1)','Bearing cap (1)','Bearing cap (1)',(#11187));
#11196=PRODUCT('Cap Screw - M5x20','Cap Screw - M5x20',
'Cap Screw - M5x20',(#11187));
#11197=PRODUCT('Sealed Ball Bearing - 10 x 30 x 9 mm',
'Sealed Ball Bearing - 10 x 30 x 9 mm',
'Sealed Ball Bearing - 10 x 30 x 9 mm',(#11187));
#11198=PRODUCT('Inner ring','Inner ring','Inner ring',(#11187));
#11199=PRODUCT('Outer ring','Outer ring','Outer ring',(#11187));
#11200=PRODUCT('Balls','Balls','Balls',(#11187));
#11201=PRODUCT('Cage','Cage','Cage',(#11187));
#11202=PRODUCT('Seals 2RS','Seals 2RS','Seals 2RS',(#11187));
#11203=PRODUCT('Input crank and locking cam',
'Input crank and locking cam','Input crank and locking cam',(#11187));
#11204=PRODUCT('Input crank and spindle','Input crank and spindle',
'Input crank and spindle',(#11187));
#11205=PRODUCT('Lower bearing sleeve','Lower bearing sleeve',
'Lower bearing sleeve',(#11187));
#11206=PRODUCT('Retaining collar','Retaining collar','Retaining collar',
(#11187));
#11207=PRODUCT('Drive pin','Drive pin','Drive pin',(#11187));
#11208=PRODUCT('Locking cam','Locking cam','Locking cam',(#11187));
#11209=PRODUCT('Locking cam spacer','Locking cam spacer',
'Locking cam spacer',(#11187));
#11210=PRODUCT('Cam keeper','Cam keeper','Cam keeper',(#11187));
#11211=PRODUCT('Crank grip','Crank grip','Crank grip',(#11187));
#11212=PRODUCT('M4x10 Cap Screw','M4x10 Cap Screw','M4x10 Cap Screw',(#11187));
#11213=PRODUCT('Four-slot output wheel','Four-slot output wheel',
'Four-slot output wheel',(#11187));
#11214=PRODUCT('Output wheel and spindle','Output wheel and spindle',
'Output wheel and spindle',(#11187));
#11215=PRODUCT('Lower bearing sleeve (1)','Lower bearing sleeve (1)',
'Lower bearing sleeve (1)',(#11187));
#11216=PRODUCT('Retaining collar (1)','Retaining collar (1)',
'Retaining collar (1)',(#11187));
#11217=PRODUCT('M4x4 collar screw','M4x4 collar screw',
'M4x4 collar screw',(#11187));
#11218=PRESENTATION_STYLE_ASSIGNMENT((#11224));
#11219=PRESENTATION_STYLE_ASSIGNMENT((#11225));
#11220=PRESENTATION_STYLE_ASSIGNMENT((#11226));
#11221=PRESENTATION_STYLE_ASSIGNMENT((#11227));
#11222=PRESENTATION_STYLE_ASSIGNMENT((#11228));
#11223=PRESENTATION_STYLE_ASSIGNMENT((#11229));
#11224=SURFACE_STYLE_USAGE(.BOTH.,#11230);
#11225=SURFACE_STYLE_USAGE(.BOTH.,#11231);
#11226=SURFACE_STYLE_USAGE(.BOTH.,#11232);
#11227=SURFACE_STYLE_USAGE(.BOTH.,#11233);
#11228=SURFACE_STYLE_USAGE(.BOTH.,#11234);
#11229=SURFACE_STYLE_USAGE(.BOTH.,#11235);
#11230=SURFACE_SIDE_STYLE('',(#11236));
#11231=SURFACE_SIDE_STYLE('',(#11237));
#11232=SURFACE_SIDE_STYLE('',(#11238));
#11233=SURFACE_SIDE_STYLE('',(#11239));
#11234=SURFACE_SIDE_STYLE('',(#11240));
#11235=SURFACE_SIDE_STYLE('',(#11241));
#11236=SURFACE_STYLE_FILL_AREA(#11242);
#11237=SURFACE_STYLE_FILL_AREA(#11243);
#11238=SURFACE_STYLE_FILL_AREA(#11244);
#11239=SURFACE_STYLE_FILL_AREA(#11245);
#11240=SURFACE_STYLE_FILL_AREA(#11246);
#11241=SURFACE_STYLE_FILL_AREA(#11247);
#11242=FILL_AREA_STYLE('Steel - Satin',(#11248));
#11243=FILL_AREA_STYLE('CAD Library Painted - Deep blue',(#11249));
#11244=FILL_AREA_STYLE('CAD Library Painted - Steel gray',(#11250));
#11245=FILL_AREA_STYLE('CAD Library Painted - Graphite',(#11251));
#11246=FILL_AREA_STYLE('CAD Library Painted - Engineering blue',(#11252));
#11247=FILL_AREA_STYLE('CAD Library Painted - Light blue',(#11253));
#11248=FILL_AREA_STYLE_COLOUR('Steel - Satin',#11254);
#11249=FILL_AREA_STYLE_COLOUR('CAD Library Painted - Deep blue',#11255);
#11250=FILL_AREA_STYLE_COLOUR('CAD Library Painted - Steel gray',#11256);
#11251=FILL_AREA_STYLE_COLOUR('CAD Library Painted - Graphite',#11257);
#11252=FILL_AREA_STYLE_COLOUR('CAD Library Painted - Engineering blue',
#11258);
#11253=FILL_AREA_STYLE_COLOUR('CAD Library Painted - Light blue',#11259);
#11254=COLOUR_RGB('Steel - Satin',0.627450980392157,0.627450980392157,0.627450980392157);
#11255=COLOUR_RGB('CAD Library Painted - Deep blue',0.0784313725490196,
0.203921568627451,0.349019607843137);
#11256=COLOUR_RGB('CAD Library Painted - Steel gray',0.592156862745098,
0.631372549019608,0.67843137254902);
#11257=COLOUR_RGB('CAD Library Painted - Graphite',0.168627450980392,0.192156862745098,
0.231372549019608);
#11258=COLOUR_RGB('CAD Library Painted - Engineering blue',0.12156862745098,
0.356862745098039,0.6);
#11259=COLOUR_RGB('CAD Library Painted - Light blue',0.286274509803922,
0.552941176470588,0.780392156862745);
#11260=COLOUR_RGB('Dark Blue',0.08,0.2,0.34);
#11261=FILL_AREA_STYLE_COLOUR('',#11260);
#11262=FILL_AREA_STYLE('',(#11261));
#11263=SURFACE_STYLE_FILL_AREA(#11262);
#11264=SURFACE_SIDE_STYLE('',(#11263));
#11265=SURFACE_STYLE_USAGE(.BOTH.,#11264);
#11266=PRESENTATION_STYLE_ASSIGNMENT((#11265));
#11267=COLOUR_RGB('Light Blue',0.38,0.62,0.78);
#11268=FILL_AREA_STYLE_COLOUR('',#11267);
#11269=FILL_AREA_STYLE('',(#11268));
#11270=SURFACE_STYLE_FILL_AREA(#11269);
#11271=SURFACE_SIDE_STYLE('',(#11270));
#11272=SURFACE_STYLE_USAGE(.BOTH.,#11271);
#11273=PRESENTATION_STYLE_ASSIGNMENT((#11272));
#11274=COLOUR_RGB('Sky Blue',0.24,0.69,0.87);
#11275=FILL_AREA_STYLE_COLOUR('',#11274);
#11276=FILL_AREA_STYLE('',(#11275));
#11277=SURFACE_STYLE_FILL_AREA(#11276);
#11278=SURFACE_SIDE_STYLE('',(#11277));
#11279=SURFACE_STYLE_USAGE(.BOTH.,#11278);
#11280=PRESENTATION_STYLE_ASSIGNMENT((#11279));
#11281=COLOUR_RGB('Grey',0.48,0.52,0.57);
#11282=FILL_AREA_STYLE_COLOUR('',#11281);
#11283=FILL_AREA_STYLE('',(#11282));
#11284=SURFACE_STYLE_FILL_AREA(#11283);
#11285=SURFACE_SIDE_STYLE('',(#11284));
#11286=SURFACE_STYLE_USAGE(.BOTH.,#11285);
#11287=PRESENTATION_STYLE_ASSIGNMENT((#11286));
#11288=COLOUR_RGB('Black',0.12,0.14,0.17);
#11289=FILL_AREA_STYLE_COLOUR('',#11288);
#11290=FILL_AREA_STYLE('',(#11289));
#11291=SURFACE_STYLE_FILL_AREA(#11290);
#11292=SURFACE_SIDE_STYLE('',(#11291));
#11293=SURFACE_STYLE_USAGE(.BOTH.,#11292);
#11294=PRESENTATION_STYLE_ASSIGNMENT((#11293));
#11295=COLOUR_RGB('Off White',0.89,0.88,0.83);
#11296=FILL_AREA_STYLE_COLOUR('',#11295);
#11297=FILL_AREA_STYLE('',(#11296));
#11298=SURFACE_STYLE_FILL_AREA(#11297);
#11299=SURFACE_SIDE_STYLE('',(#11298));
#11300=SURFACE_STYLE_USAGE(.BOTH.,#11299);
#11301=PRESENTATION_STYLE_ASSIGNMENT((#11300));
ENDSEC;
END-ISO-10303-21;
